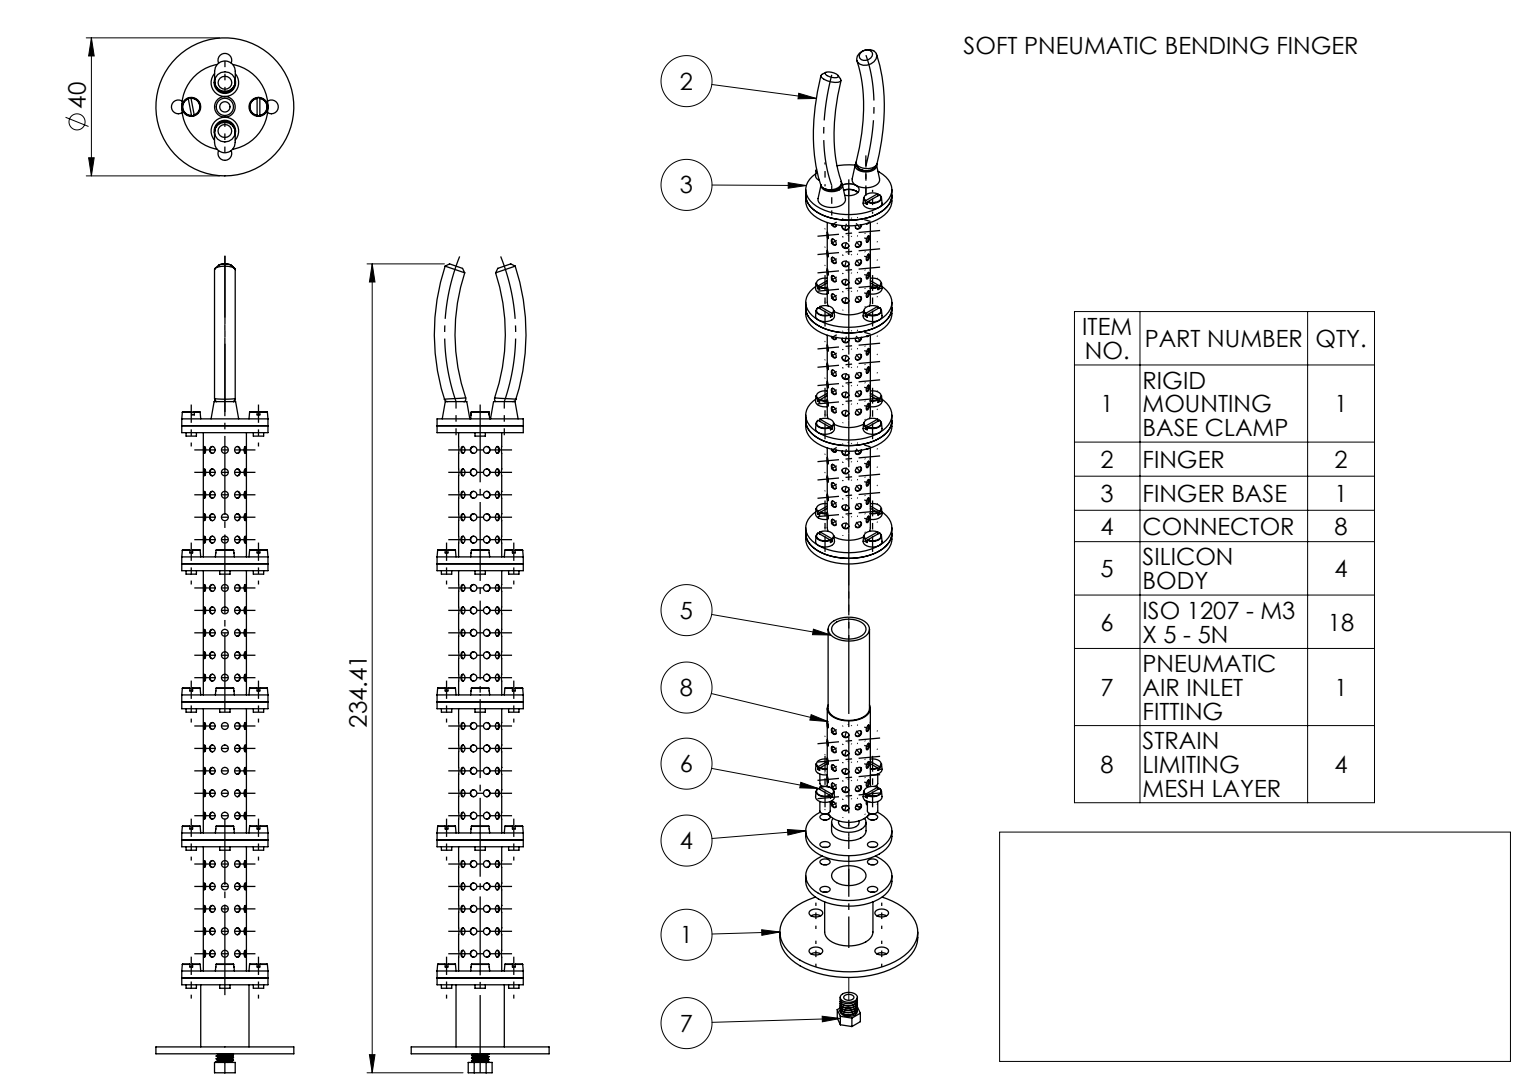
ISO-10303-21;
HEADER;
FILE_DESCRIPTION (('STEP AP214'),
    '1' );
FILE_NAME ('BR-012',
    '2026-10-04T10:31:01',
    ( '' ),
    ( '' ),
    'SwSTEP 2.0',
    'SolidWorks 2026',
    '' );
FILE_SCHEMA (( 'AUTOMOTIVE_DESIGN' ));
ENDSEC;

DATA;
#1 = DIRECTION ( 'NONE',  ( 1.251928832280965695E-16, 1.000000000000000000, 0.000000000000000000 ) ) ;
#2 = CARTESIAN_POINT ( 'NONE',  ( -5.408775798201173046, 2.598833957129639494, 10.88602261056916554 ) ) ;
#3 = CARTESIAN_POINT ( 'NONE',  ( 5.866817325727491372, 1.260653813892048003, 4.199777826161211536 ) ) ;
#4 = CARTESIAN_POINT ( 'NONE',  ( -5.621278735166248097, 2.101423246382425614, 30.02591947216899015 ) ) ;
#5 = ORIENTED_EDGE ( 'NONE', *, *, #943, .F. ) ;
#6 = ADVANCED_FACE ( 'NONE', ( #14827 ), #6324, .F. ) ;
#7 = VECTOR ( 'NONE', #2853, 1000.000000000000000 ) ;
#8 = ORIENTED_EDGE ( 'NONE', *, *, #4476, .T. ) ;
#9 = ORIENTED_EDGE ( 'NONE', *, *, #12350, .T. ) ;
#10 = LINE ( 'NONE', #5828, #1733 ) ;
#11 = EDGE_CURVE ( 'NONE', #6555, #15690, #9827, .T. ) ;
#12 = EDGE_LOOP ( 'NONE', ( #2014, #1529, #7352, #6634 ) ) ;
#13 = CARTESIAN_POINT ( 'NONE',  ( -1.461580736456472795, 1.461580736456472795, 1.150000001092474688 ) ) ;
#14 = DIRECTION ( 'NONE',  ( 0.000000000000000000, -0.000000000000000000, 1.000000000000000000 ) ) ;
#15 = DIRECTION ( 'NONE',  ( 0.000000000000000000, 1.000000000000000000, 0.000000000000000000 ) ) ;
#16 = CARTESIAN_POINT ( 'NONE',  ( 0.8561741729129460632, 185.8999999989075036, 9.066987299999999195 ) ) ;
#17 = CARTESIAN_POINT ( 'NONE',  ( 2.500000000000000000, 3.061616997868383141E-16, 2.100000000000000089 ) ) ;
#18 = LINE ( 'NONE', #14576, #2348 ) ;
#19 = ITEM_DEFINED_TRANSFORMATION ( 'NONE', 'NONE', #1959,  #14201 ) ;
#20 = FACE_OUTER_BOUND ( 'NONE', #6226, .T. ) ;
#21 = CARTESIAN_POINT ( 'NONE',  ( 0.8561741729129451750, 2.066987299999999639, 2.000000001092475443 ) ) ;
#22 = CARTESIAN_POINT ( 'NONE',  ( -3.061616997868391523E-16, 189.0000000000000000, -7.000000000000000000 ) ) ;
#23 = CARTESIAN_POINT ( 'NONE',  ( -2.191511056945971259, 226.6300844452854903, 5.385369267317587472 ) ) ;
#24 = CARTESIAN_POINT ( 'NONE',  ( 6.081836621194421255, 1.445163676684907417, 5.873058915543010627 ) ) ;
#25 = VERTEX_POINT ( 'NONE', #11007 ) ;
#26 = VERTEX_POINT ( 'NONE', #13779 ) ;
#27 = EDGE_LOOP ( 'NONE', ( #6618, #1977 ) ) ;
#28 = VERTEX_POINT ( 'NONE', #11082 ) ;
#29 = CARTESIAN_POINT ( 'NONE',  ( 8.572527594031473190E-16, 19.99999999999999645, 7.000000000000000000 ) ) ;
#30 = DIRECTION ( 'NONE',  ( 0.000000000000000000, 1.000000000000000000, 0.000000000000000000 ) ) ;
#31 = CARTESIAN_POINT ( 'NONE',  ( -2.499999999999998224, 185.2500000000000284, 8.035533905932741305 ) ) ;
#32 = CARTESIAN_POINT ( 'NONE',  ( -6.176542424588117974, 0.9554180641285662245, 31.13234125634169658 ) ) ;
#33 = CARTESIAN_POINT ( 'NONE',  ( -2.500000000000000444, 185.8999999978150584, 7.000000000000000000 ) ) ;
#34 = CARTESIAN_POINT ( 'NONE',  ( -3.107583187530418289, -5.133966411712689748, 12.37380682714709401 ) ) ;
#35 = CARTESIAN_POINT ( 'NONE',  ( -5.769755079862331826, 2.405651898698942581, 5.873058915543010627 ) ) ;
#36 = CARTESIAN_POINT ( 'NONE',  ( -6.176542424588075342, -0.9554180641288342324, 24.36765874365829987 ) ) ;
#37 = CARTESIAN_POINT ( 'NONE',  ( 0.9999502950804096679, -5.916088184763849789, 24.63108149190011176 ) ) ;
#38 = CARTESIAN_POINT ( 'NONE',  ( 0.000000000000000000, 22.00000000000000000, 0.000000000000000000 ) ) ;
#39 = CARTESIAN_POINT ( 'NONE',  ( -1.767766952966369320, 186.5999999978150754, 5.232233047033630235 ) ) ;
#40 = CARTESIAN_POINT ( 'NONE',  ( 2.467000123265670641, 227.8390626820829823, 8.944723654098295285 ) ) ;
#41 = FACE_BOUND ( 'NONE', #6027, .T. ) ;
#42 = EDGE_CURVE ( 'NONE', #14222, #12950, #1605, .T. ) ;
#43 = CARTESIAN_POINT ( 'NONE',  ( -2.367714804004699136, 189.3873339094368191, 5.166511778942795452 ) ) ;
#44 = EDGE_LOOP ( 'NONE', ( #13948, #7274 ) ) ;
#45 = CARTESIAN_POINT ( 'NONE',  ( 0.000000000000000000, 22.00000000000000000, -5.000000000000000000 ) ) ;
#46 = FACE_OUTER_BOUND ( 'NONE', #102, .T. ) ;
#47 = CARTESIAN_POINT ( 'NONE',  ( 7.799024015210693328, -1.482594289696895551, 24.49999999999999289 ) ) ;
#48 = LINE ( 'NONE', #2436, #232 ) ;
#49 = DIRECTION ( 'NONE',  ( -1.000000000000000000, 0.000000000000000000, 0.000000000000000000 ) ) ;
#50 = CARTESIAN_POINT ( 'NONE',  ( -3.420311045507875125, 4.931422832349270813, 10.49992038825521767 ) ) ;
#51 = EDGE_CURVE ( 'NONE', #13172, #10136, #3947, .T. ) ;
#52 = CARTESIAN_POINT ( 'NONE',  ( 1.461580736456473018, -1.461580736456472573, -0.6499999989075253559 ) ) ;
#53 = LINE ( 'NONE', #4919, #15568 ) ;
#54 = DIRECTION ( 'NONE',  ( 0.000000000000000000, 0.000000000000000000, 1.000000000000000000 ) ) ;
#55 = CARTESIAN_POINT ( 'NONE',  ( -1.767766952966369765, 186.8300000002185186, 8.767766952966368876 ) ) ;
#56 = CARTESIAN_POINT ( 'NONE',  ( -4.070051655338111196, 4.744673454622471809, 5.873673286359928802 ) ) ;
#57 = CARTESIAN_POINT ( 'NONE',  ( 1.989910900261709470, 228.2393533748197569, 6.930657055068108363 ) ) ;
#58 = CARTESIAN_POINT ( 'NONE',  ( 0.8561741729129452860, 2.066987299999999639, 2.000000001092474999 ) ) ;
#59 = VECTOR ( 'NONE', #8000, 1000.000000000000000 ) ;
#60 = CARTESIAN_POINT ( 'NONE',  ( 5.558508435838322548, -2.857531096718671115, 24.49999999999999289 ) ) ;
#61 = ORIENTED_EDGE ( 'NONE', *, *, #6502, .F. ) ;
#62 = DIRECTION ( 'NONE',  ( -0.5877852522924685852, -0.8090169943749507819, 0.000000000000000000 ) ) ;
#63 = PRODUCT_DEFINITION_SHAPE ( 'NONE', 'NONE',  #15745 ) ;
#64 = CARTESIAN_POINT ( 'NONE',  ( -0.8561741729129470624, 185.5999999989075206, 9.066987300000000971 ) ) ;
#65 = DIRECTION ( 'NONE',  ( 1.000000000000000000, 0.000000000000000000, 0.000000000000000000 ) ) ;
#67 = ORIENTED_EDGE ( 'NONE', *, *, #457, .F. ) ;
#66 = CARTESIAN_POINT ( 'NONE',  ( 3.566234721238059624, 5.134387337253815353, 30.00008258189710730 ) ) ;
#68 = EDGE_CURVE ( 'NONE', #7891, #15426, #13595, .T. ) ;
#69 = CARTESIAN_POINT ( 'NONE',  ( 0.6151877315911880029, -6.220340188095996758, 25.29906673469669443 ) ) ;
#70 = EDGE_CURVE ( 'NONE', #13541, #6298, #6755, .T. ) ;
#71 = CARTESIAN_POINT ( 'NONE',  ( 2.817313151350924638, 5.579000502529565253, 24.49999999999999289 ) ) ;
#72 = DIRECTION ( 'NONE',  ( -0.5877852522924685852, -0.8090169943749508930, 0.000000000000000000 ) ) ;
#73 = CARTESIAN_POINT ( 'NONE',  ( -1.732476358310940601, 189.0000000000000853, 8.805961798289683173 ) ) ;
#74 = CARTESIAN_POINT ( 'NONE',  ( 4.005785023174416537, -4.467917056767432449, 18.79952054102714243 ) ) ;
#75 = CARTESIAN_POINT ( 'NONE',  ( -2.500000000000000000, 0.000000000000000000, -2.199999997815050623 ) ) ;
#76 = CARTESIAN_POINT ( 'NONE',  ( -0.9737778612005270062, -5.920671847850523584, 30.73736375884650585 ) ) ;
#77 = LINE ( 'NONE', #5895, #15592 ) ;
#78 = EDGE_CURVE ( 'NONE', #4035, #7910, #13252, .T. ) ;
#79 = CARTESIAN_POINT ( 'NONE',  ( -0.9740012993918838458, -6.173846968979659344, 18.26164920628437471 ) ) ;
#80 = CYLINDRICAL_SURFACE ( 'NONE', #3453, 2.000000000000000000 ) ;
#81 = CARTESIAN_POINT ( 'NONE',  ( 0.000000000000000000, 0.000000000000000000, -5.500000000000000000 ) ) ;
#82 = ORIENTED_EDGE ( 'NONE', *, *, #7980, .T. ) ;
#83 = B_SPLINE_CURVE_WITH_KNOTS ( 'NONE', 3,
 ( #5175, #14802, #5099, #8688, #8760, #13593, #1502, #6378, #11290, #544, #7481, #9951, #10027, #7789, #7554, #1580, #2625, #11212 ),
 .UNSPECIFIED., .F., .F.,
 ( 4, 2, 2, 2, 2, 2, 2, 2, 4 ),
 ( 0.000000000000000000, 0.0003914898357794967363, 0.0007829796715589934725, 0.001174469507338490263, 0.001565959343117986945, 0.001957449178897483627, 0.002348939014676980526, 0.002740428850456476991, 0.003131918686235973890 ),
 .UNSPECIFIED. ) ;
#84 = ORIENTED_EDGE ( 'NONE', *, *, #4688, .F. ) ;
#85 = ORIENTED_EDGE ( 'NONE', *, *, #14143, .F. ) ;
#86 = CARTESIAN_POINT ( 'NONE',  ( -2.692215568229989753, 5.362327947133520567, 24.76229037835931734 ) ) ;
#87 = ORIENTED_EDGE ( 'NONE', *, *, #14600, .T. ) ;
#88 = CARTESIAN_POINT ( 'NONE',  ( -1.035533905932737753, 2.500000000000000444, -1.549999997815050490 ) ) ;
#89 = CARTESIAN_POINT ( 'NONE',  ( 5.903472034603520768, 2.056448723545130974, 19.00008219321555103 ) ) ;
#90 = CARTESIAN_POINT ( 'NONE',  ( 6.106056299406735555, 1.336851112280737386, 31.79887838423339730 ) ) ;
#91 = CARTESIAN_POINT ( 'NONE',  ( -1.461580736456473018, 188.7499999989075263, 5.538419263543527649 ) ) ;
#92 = EDGE_CURVE ( 'NONE', #15044, #5826, #4325, .T. ) ;
#93 = AXIS2_PLACEMENT_3D ( 'NONE', #6041, #2604, #1097 ) ;
#94 = CARTESIAN_POINT ( 'NONE',  ( -1.530808498934191571E-16, 2.500000000000000000, 0.6999999999999998446 ) ) ;
#95 = LINE ( 'NONE', #7268, #828 ) ;
#96 = CONTEXT_DEPENDENT_SHAPE_REPRESENTATION ( #10266, #5907 ) ;
#97 = CARTESIAN_POINT ( 'NONE',  ( 3.421280866381150698, 4.930711975950905490, 6.000049320733126024 ) ) ;
#98 = CARTESIAN_POINT ( 'NONE',  ( 2.066987299999999639, 0.8561741729129456191, -2.299999998907525711 ) ) ;
#99 = CARTESIAN_POINT ( 'NONE',  ( 4.435347140101059793, -4.403429997944484420, 30.86762589283693714 ) ) ;
#100 = CARTESIAN_POINT ( 'NONE',  ( -2.809196860006122787, 226.9495188873497966, 6.326437523183426670 ) ) ;
#101 = DIRECTION ( 'NONE',  ( 0.000000000000000000, 0.000000000000000000, -1.000000000000000000 ) ) ;
#102 = EDGE_LOOP ( 'NONE', ( #11466, #15646, #12937, #12328 ) ) ;
#103 = EDGE_LOOP ( 'NONE', ( #8397, #1444 ) ) ;
#104 = EDGE_LOOP ( 'NONE', ( #9975, #181, #5986, #469 ) ) ;
#105 = CARTESIAN_POINT ( 'NONE',  ( 1.354942165200771727E-13, 6.000000000000000888, 16.99999999999998579 ) ) ;
#106 = CARTESIAN_POINT ( 'NONE',  ( 1.753917783834456179, 189.0000000000000568, 8.787807858281036388 ) ) ;
#107 = CARTESIAN_POINT ( 'NONE',  ( 7.347880431581855163E-16, -6.250000000000000888, 4.000000000000004441 ) ) ;
#108 = CARTESIAN_POINT ( 'NONE',  ( 3.010624175977998807, -5.190832888732208161, 12.29888242247939623 ) ) ;
#109 = VECTOR ( 'NONE', #6035, 1000.000000000000114 ) ;
#110 = UNCERTAINTY_MEASURE_WITH_UNIT (LENGTH_MEASURE( 1.000000000000000082E-05 ), #6665, 'distance_accuracy_value', 'NONE');
#111 = CARTESIAN_POINT ( 'NONE',  ( 0.5042987395408317086, 5.979983180450071600, 12.37329304179975509 ) ) ;
#112 = CARTESIAN_POINT ( 'NONE',  ( -0.2637975869345823843, -6.245592211692903462, 25.47332839949191197 ) ) ;
#113 = EDGE_CURVE ( 'NONE', #5247, #7816, #14877, .T. ) ;
#114 = CARTESIAN_POINT ( 'NONE',  ( -5.858813228503674253, 2.179803269293212331, 5.973772828752684561 ) ) ;
#115 = CARTESIAN_POINT ( 'NONE',  ( 5.931828553037963303, 0.9033193133619970006, 30.73805675996854703 ) ) ;
#116 = DIRECTION ( 'NONE',  ( -6.123233995736766036E-17, 1.000000000000000000, 0.000000000000000000 ) ) ;
#117 = CARTESIAN_POINT ( 'NONE',  ( 0.000000000000000000, 102.0000000000000142, 0.000000000000000000 ) ) ;
#118 = CARTESIAN_POINT ( 'NONE',  ( -7.826584432629735133E-16, 189.2999999978150356, 9.500000000000001776 ) ) ;
#119 = CARTESIAN_POINT ( 'NONE',  ( 1.829800800964088481, 226.5245823332902546, 5.074452397578279594 ) ) ;
#120 = CARTESIAN_POINT ( 'NONE',  ( 5.866817325727508248, 1.260653813891974062, 10.69977782616119732 ) ) ;
#121 = CARTESIAN_POINT ( 'NONE',  ( -2.425137606382978372, 188.9999999978561505, 7.628313597219490205 ) ) ;
#122 = EDGE_LOOP ( 'NONE', ( #8457, #957, #1817, #14670 ) ) ;
#123 = CARTESIAN_POINT ( 'NONE',  ( -3.735642931251032639, 4.696778275484473575, 5.974080527831013399 ) ) ;
#124 = DIRECTION ( 'NONE',  ( -0.3090169943749584980, 0.9510565162951498674, 0.000000000000000000 ) ) ;
#125 = CARTESIAN_POINT ( 'NONE',  ( 0.000000000000000000, 6.250000000000000888, 25.49999999999999645 ) ) ;
#126 = CARTESIAN_POINT ( 'NONE',  ( 0.5031281619709804254, 5.980084330432649864, 23.62602272744524967 ) ) ;
#127 = CARTESIAN_POINT ( 'NONE',  ( 0.000000000000000000, 184.0000000000000000, 0.000000000000000000 ) ) ;
#128 = CARTESIAN_POINT ( 'NONE',  ( -2.782769401326250058, 5.315896561274810139, 10.99571079637980553 ) ) ;
#129 = CARTESIAN_POINT ( 'NONE',  ( 3.796994071234844259E-16, -2.066987299999999639, 0.8500000010924748661 ) ) ;
#130 = CARTESIAN_POINT ( 'NONE',  ( 5.621197618055712830, -2.101623592078416980, 4.026019798777604741 ) ) ;
#131 = AXIS2_PLACEMENT_3D ( 'NONE', #7436, #13712, #10064 ) ;
#132 = LINE ( 'NONE', #11034, #13057 ) ;
#133 = CARTESIAN_POINT ( 'NONE',  ( -2.500000000000000444, 186.7300000002184959, 7.000000000000000000 ) ) ;
#134 = CARTESIAN_POINT ( 'NONE',  ( -2.500000000000000000, 0.000000000000000000, -2.199999997815050623 ) ) ;
#135 = CARTESIAN_POINT ( 'NONE',  ( 0.000000000000000000, 2.000000000000000000, -5.000000000000000000 ) ) ;
#136 = CARTESIAN_POINT ( 'NONE',  ( 0.8561741729129452860, 2.066987299999999639, -1.199999998907525178 ) ) ;
#137 = CARTESIAN_POINT ( 'NONE',  ( 0.7995298244854847081, 5.947211616899245712, 31.61456014619858834 ) ) ;
#138 = EDGE_LOOP ( 'NONE', ( #2074, #6168, #2631, #14050 ) ) ;
#139 = CARTESIAN_POINT ( 'NONE',  ( 0.8561741729129465073, -2.066987299999999195, 0.7000000010924749549 ) ) ;
#140 = CARTESIAN_POINT ( 'NONE',  ( -1.461580736456473906, 186.3499999989074922, 8.461580736456474128 ) ) ;
#141 = CARTESIAN_POINT ( 'NONE',  ( -4.290821322214377176, -4.545321419741554791, 12.11441947245482886 ) ) ;
#142 = VECTOR ( 'NONE', #3301, 1000.000000000000114 ) ;
#144 = ORIENTED_EDGE ( 'NONE', *, *, #8868, .F. ) ;
#143 = CARTESIAN_POINT ( 'NONE',  ( 8.809142651444723526E-17, 184.6499999989075320, 4.933012699999999029 ) ) ;
#145 = CYLINDRICAL_SURFACE ( 'NONE', #13956, 1.000000000000000888 ) ;
#146 = LINE ( 'NONE', #13353, #5536 ) ;
#147 = DIRECTION ( 'NONE',  ( -1.000000000000000000, 0.000000000000000000, 0.000000000000000000 ) ) ;
#148 = B_SPLINE_CURVE_WITH_KNOTS ( 'NONE', 1,
 ( #12898, #4831 ),
 .UNSPECIFIED., .F., .F.,
 ( 2, 2 ),
 ( 0.000000000000000000, 1.000000000000000000 ),
 .UNSPECIFIED. ) ;
#149 = DIRECTION ( 'NONE',  ( 0.8090169943749421222, 0.5877852522924802425, 0.000000000000000000 ) ) ;
#150 = CARTESIAN_POINT ( 'NONE',  ( 1.461580736456472573, 188.9499999989075150, 8.461580736456474128 ) ) ;
#151 = CARTESIAN_POINT ( 'NONE',  ( 5.782895619916224028, -1.604017620857841386, 25.47408052783099919 ) ) ;
#152 = CARTESIAN_POINT ( 'NONE',  ( -13.50000000000000000, -0.001000000000000132727, -1.999999999999997113 ) ) ;
#153 = CARTESIAN_POINT ( 'NONE',  ( -1.000079958708118610, -5.916066267613704355, 31.13152738882033788 ) ) ;
#154 = CARTESIAN_POINT ( 'NONE',  ( 5.621197618055728817, -2.101623592078373903, 10.52601979877759142 ) ) ;
#155 = CARTESIAN_POINT ( 'NONE',  ( -4.435347140101089103, 4.403429997944455110, 31.00000000000000000 ) ) ;
#156 = CARTESIAN_POINT ( 'NONE',  ( 12.50000000000000533, 1.530808498934192113E-15, 0.000000000000000000 ) ) ;
#157 = CARTESIAN_POINT ( 'NONE',  ( -5.935543223013860725, 0.8771126767606856056, 30.86760611998365178 ) ) ;
#158 = EDGE_CURVE ( 'NONE', #3364, #642, #4897, .T. ) ;
#159 = VERTEX_POINT ( 'NONE', #1682 ) ;
#160 = EDGE_CURVE ( 'NONE', #4150, #13293, #5091, .T. ) ;
#161 = ORIENTED_EDGE ( 'NONE', *, *, #15144, .T. ) ;
#162 = ORIENTED_EDGE ( 'NONE', *, *, #10171, .F. ) ;
#163 = CARTESIAN_POINT ( 'NONE',  ( -5.329907877631262281, -2.755840666746435019, 24.76194324003146008 ) ) ;
#164 = VECTOR ( 'NONE', #7946, 1000.000000000000000 ) ;
#165 = ORIENTED_EDGE ( 'NONE', *, *, #10559, .T. ) ;
#166 = PRODUCT ( 'finger base', 'finger base', '', ( #15382 ) ) ;
#167 = CARTESIAN_POINT ( 'NONE',  ( -1.461580736456472351, -1.461580736456473018, -0.2499999989075251672 ) ) ;
#168 = FACE_BOUND ( 'NONE', #3506, .T. ) ;
#169 = DIRECTION ( 'NONE',  ( 0.000000000000000000, 0.000000000000000000, 1.000000000000000000 ) ) ;
#170 = DIRECTION ( 'NONE',  ( -1.000000000000000000, 3.326610055774637112E-18, 1.062480551894331163E-17 ) ) ;
#171 = CARTESIAN_POINT ( 'NONE',  ( 1.767766952966369320, -1.767766952966368654, 2.000000000000000000 ) ) ;
#172 = CARTESIAN_POINT ( 'NONE',  ( -5.558508435838229289, 2.857531096718854524, 5.000000000000004441 ) ) ;
#173 = CONTEXT_DEPENDENT_SHAPE_REPRESENTATION ( #5992, #5517 ) ;
#174 = CARTESIAN_POINT ( 'NONE',  ( 2.668367453516629517, 5.373994336898131330, 5.130649613488545313 ) ) ;
#175 = CARTESIAN_POINT ( 'NONE',  ( 2.066987300000000083, -0.8561741729129449530, -0.7999999989075252671 ) ) ;
#176 = CARTESIAN_POINT ( 'NONE',  ( 0.000000000000000000, 0.000000000000000000, 5.000000000000004441 ) ) ;
#177 = CARTESIAN_POINT ( 'NONE',  ( -2.923025936753522291, 227.5090509392885281, 7.973756422523831766 ) ) ;
#178 = EDGE_CURVE ( 'NONE', #5942, #5121, #706, .T. ) ;
#179 = ORIENTED_EDGE ( 'NONE', *, *, #8379, .T. ) ;
#180 = ORIENTED_EDGE ( 'NONE', *, *, #12545, .T. ) ;
#181 = ORIENTED_EDGE ( 'NONE', *, *, #13568, .T. ) ;
#182 = DIRECTION ( 'NONE',  ( -0.1736481776669306920, -0.9848077530122080203, 0.000000000000000000 ) ) ;
#183 = LINE ( 'NONE', #11083, #4538 ) ;
#184 = B_SPLINE_CURVE_WITH_KNOTS ( 'NONE', 3,
 ( #1419, #11210, #385, #5255, #7552, #10102, #6529, #6608, #14955, #11441, #11134, #235, #4046, #5097, #5411, #8917, #12556, #1655 ),
 .UNSPECIFIED., .F., .F.,
 ( 4, 2, 2, 2, 2, 2, 2, 2, 4 ),
 ( 0.003131918686235975625, 0.003523310662250265894, 0.003914702638264556597, 0.004306094614278846433, 0.004697486590293137136, 0.005088878566307427839, 0.005480270542321717675, 0.005871662518336007511, 0.006263054494350298214 ),
 .UNSPECIFIED. ) ;
#185 = CARTESIAN_POINT ( 'NONE',  ( 6.123233995736766282E-16, -6.000000000000000888, 6.000000000000005329 ) ) ;
#186 = CARTESIAN_POINT ( 'NONE',  ( 0.1306394121200732117, -6.249999999999998224, 16.99999999999998934 ) ) ;
#187 = DIRECTION ( 'NONE',  ( 0.8660254037844385966, 0.4999999999999998890, 0.000000000000000000 ) ) ;
#188 = DIRECTION ( 'NONE',  ( 0.000000000000000000, 0.000000000000000000, 1.000000000000000000 ) ) ;
#189 = DIRECTION ( 'NONE',  ( -0.5877852522924685852, -0.8090169943749508930, 0.000000000000000000 ) ) ;
#190 = CARTESIAN_POINT ( 'NONE',  ( 5.486982057989218120, -2.429327048029818137, 12.29931806258173488 ) ) ;
#191 = CARTESIAN_POINT ( 'NONE',  ( -7.799024015210622274, -1.482594289697344969, 17.99999999999998934 ) ) ;
#192 = CARTESIAN_POINT ( 'NONE',  ( 6.805491029613696752E-14, 66.00000000000000000, -9.750000000000003553 ) ) ;
#193 = B_SPLINE_CURVE_WITH_KNOTS ( 'NONE', 3,
 ( #6450, #7867, #11284, #4121, #12707, #459, #1650 ),
 .UNSPECIFIED., .F., .F.,
 ( 4, 3, 4 ),
 ( 0.004471049636504374758, 0.004805482912052319762, 0.005232732616948215093 ),
 .UNSPECIFIED. ) ;
#194 = CARTESIAN_POINT ( 'NONE',  ( 4.404571325722361763E-17, 185.7699999975965568, 4.500000000000000000 ) ) ;
#195 = CARTESIAN_POINT ( 'NONE',  ( -1.740752211025599738, 227.9442165381023528, 6.078285037125840340 ) ) ;
#196 = CARTESIAN_POINT ( 'NONE',  ( 2.789580270747262780, 227.6450226773988845, 8.373868502673408543 ) ) ;
#197 = CARTESIAN_POINT ( 'NONE',  ( 0.3061381340472814627, 189.0451911194899424, 10.17413847366682234 ) ) ;
#198 =( REPRESENTATION_RELATIONSHIP ('NONE','NONE', #11191, #3660 ) REPRESENTATION_RELATIONSHIP_WITH_TRANSFORMATION ( #14497 )SHAPE_REPRESENTATION_RELATIONSHIP( ) );
#199 = CIRCLE ( 'NONE', #5549, 2.499999999999999556 ) ;
#200 = CARTESIAN_POINT ( 'NONE',  ( -0.2618185962740512407, 189.0446530151151023, 10.17853758010602760 ) ) ;
#201 = EDGE_CURVE ( 'NONE', #13777, #13408, #2146, .T. ) ;
#202 = VERTEX_POINT ( 'NONE', #2611 ) ;
#203 = CARTESIAN_POINT ( 'NONE',  ( -6.176542424588105540, -0.9554180641286327269, 5.000000000000004441 ) ) ;
#204 = CARTESIAN_POINT ( 'NONE',  ( -5.859221468178929193, 2.178708437343280568, 23.52591457665828401 ) ) ;
#205 = PRODUCT_RELATED_PRODUCT_CATEGORY ( 'part', '', ( #166 ) ) ;
#206 = CARTESIAN_POINT ( 'NONE',  ( -12.50000000000000533, 0.000000000000000000, 2.000000000000001776 ) ) ;
#207 = CARTESIAN_POINT ( 'NONE',  ( 6.176542424588116198, 0.9554180641285651143, 11.63060690723497537 ) ) ;
#208 = CARTESIAN_POINT ( 'NONE',  ( 0.9639874461523436633, 228.2061259459514133, 10.02419290002115915 ) ) ;
#209 =( BOUNDED_CURVE ( )  B_SPLINE_CURVE ( 2, ( #7437, #5274, #15205, #1752, #11093, #14680, #10274, #6626, #3769 ),
 .UNSPECIFIED., .F., .F. ) 
 B_SPLINE_CURVE_WITH_KNOTS ( ( 3, 2, 2, 2, 3 ),
 ( 0.000000000000000000, 0.01785714285714285615, 0.03571428571428571230, 0.05357142857142856845, 0.07142857142857142461 ),
 .UNSPECIFIED. ) 
 CURVE ( )  GEOMETRIC_REPRESENTATION_ITEM ( )  RATIONAL_B_SPLINE_CURVE ( ( 1.000000000000000000, 0.9238795325112867385, 1.000000000000000000, 0.9238795325112867385, 1.000000000000000000, 0.9238795325112867385, 1.000000000000000000, 0.9238795325112867385, 1.000000000000000000 ) ) 
 REPRESENTATION_ITEM ( '' )  );
#210 = EDGE_CURVE ( 'NONE', #4790, #898, #15357, .T. ) ;
#211 = AXIS2_PLACEMENT_3D ( 'NONE', #13271, #4928, #12230 ) ;
#212 = CARTESIAN_POINT ( 'NONE',  ( 4.322356511625485176, 7.650514973136679941, 24.49999999999999289 ) ) ;
#213 = CARTESIAN_POINT ( 'NONE',  ( 0.8561741729129451750, 2.066987299999999639, -1.199999998907525622 ) ) ;
#214 = FACE_OUTER_BOUND ( 'NONE', #10362, .T. ) ;
#215 = SURFACE_SIDE_STYLE ('',( #11110 ) ) ;
#216 = CARTESIAN_POINT ( 'NONE',  ( -0.6144300524833441468, -6.220417338033054300, 30.20033372175933550 ) ) ;
#217 = CARTESIAN_POINT ( 'NONE',  ( -2.500000000000000444, 186.7800000002184504, 8.035533905932737753 ) ) ;
#218 = DIRECTION ( 'NONE',  ( 0.000000000000000000, 0.000000000000000000, -1.000000000000000000 ) ) ;
#219 = CARTESIAN_POINT ( 'NONE',  ( 0.8799020092372641377, 228.8451675208714562, 8.680282862240067843 ) ) ;
#220 = CARTESIAN_POINT ( 'NONE',  ( -0.8561741729129455081, 2.066987299999999639, -1.899999998907525134 ) ) ;
#221 = CARTESIAN_POINT ( 'NONE',  ( -3.567624405365271478, -5.133384272590760133, 10.50004921015705150 ) ) ;
#222 = CARTESIAN_POINT ( 'NONE',  ( -1.265664690411614835E-16, 2.066987299999999639, 0.2500000010924746663 ) ) ;
#223 = VECTOR ( 'NONE', #5063, 1000.000000000000114 ) ;
#224 = CARTESIAN_POINT ( 'NONE',  ( -2.066987300000001859, 187.8999999989075036, 7.856174172912944620 ) ) ;
#225 = CARTESIAN_POINT ( 'NONE',  ( 6.172651332693116721, -0.9815532474592382206, 18.26190213084011660 ) ) ;
#226 = EDGE_LOOP ( 'NONE', ( #14083, #11757, #15041, #247 ) ) ;
#227 = CARTESIAN_POINT ( 'NONE',  ( -3.735642931251134335, -4.696778275484388310, 23.52591947216897594 ) ) ;
#228 = CARTESIAN_POINT ( 'NONE',  ( -11.25000000000000355, 3.419666426228851687E-14, 2.000000000000001776 ) ) ;
#229 = CARTESIAN_POINT ( 'NONE',  ( 5.903596343266298341, -2.055998103990583026, 31.99995078984293428 ) ) ;
#230 = CARTESIAN_POINT ( 'NONE',  ( 5.131373506000437068, 7.062729720844210135, 24.49999999999999289 ) ) ;
#231 = CARTESIAN_POINT ( 'NONE',  ( -0.8561741729129471734, 188.7999999989075093, 9.066987300000000971 ) ) ;
#232 = VECTOR ( 'NONE', #9608, 1000.000000000000000 ) ;
#233 = CARTESIAN_POINT ( 'NONE',  ( -0.05280792143845736142, 189.0000000000001137, 9.499442202459045248 ) ) ;
#234 = CARTESIAN_POINT ( 'NONE',  ( 9.750000000000003553, 19.99999999999999645, 1.020968533498575335E-13 ) ) ;
#235 = CARTESIAN_POINT ( 'NONE',  ( 3.922396193919112317, -4.541970110199391009, 5.873806827147107334 ) ) ;
#236 = CARTESIAN_POINT ( 'NONE',  ( -5.746837578676007752, 1.729433780394243003, 10.50004946353775459 ) ) ;
#237 = CYLINDRICAL_SURFACE ( 'NONE', #3717, 2.500000000000000000 ) ;
#238 = CARTESIAN_POINT ( 'NONE',  ( 13.50000000000000000, 2.000000000000000000, -2.000000000000000444 ) ) ;
#239 = ORIENTED_EDGE ( 'NONE', *, *, #1750, .T. ) ;
#240 = CARTESIAN_POINT ( 'NONE',  ( -0.8561741729129455081, 187.0999999989075206, 4.933012699999999029 ) ) ;
#241 = ORIENTED_EDGE ( 'NONE', *, *, #4453, .T. ) ;
#242 = PLANE ( 'NONE',  #13414 ) ;
#243 = ORIENTED_EDGE ( 'NONE', *, *, #15436, .T. ) ;
#244 = AXIS2_PLACEMENT_3D ( 'NONE', #12080, #1179, #6133 ) ;
#245 = CARTESIAN_POINT ( 'NONE',  ( -2.782713018890816681, 5.315928322779066129, 25.00439760644211518 ) ) ;
#246 = CIRCLE ( 'NONE', #4794, 1.499999999999999556 ) ;
#247 = ORIENTED_EDGE ( 'NONE', *, *, #524, .F. ) ;
#248 = CARTESIAN_POINT ( 'NONE',  ( 3.796994071234844259E-16, -2.066987299999999639, -0.1499999989075253282 ) ) ;
#249 = CARTESIAN_POINT ( 'NONE',  ( 5.770288754215144422, 2.404361317819916355, 18.87381964045070859 ) ) ;
#250 = CARTESIAN_POINT ( 'NONE',  ( -2.113934160113910998, 227.9745842263959048, 9.343330332359114365 ) ) ;
#251 = CARTESIAN_POINT ( 'NONE',  ( -0.8561741729129470624, 188.9999999989074979, 9.066987299999999195 ) ) ;
#252 = CARTESIAN_POINT ( 'NONE',  ( 0.4831378333609244180, 2.500000000000000000, -2.516327958217759342 ) ) ;
#253 = ADVANCED_FACE ( 'NONE', ( #9289 ), #846, .F. ) ;
#254 = DIRECTION ( 'NONE',  ( 0.000000000000000000, 1.000000000000000000, 0.000000000000000000 ) ) ;
#255 = DIRECTION ( 'NONE',  ( 0.8090169943749421222, 0.5877852522924802425, 0.000000000000000000 ) ) ;
#256 = CARTESIAN_POINT ( 'NONE',  ( 3.796994071234844259E-16, -2.066987299999999639, 0.8500000010924748661 ) ) ;
#257 = CARTESIAN_POINT ( 'NONE',  ( -6.155867707731118799, 1.081837891425841747, 30.49563030319847101 ) ) ;
#258 = CARTESIAN_POINT ( 'NONE',  ( -2.548338711267991386, 226.7802694665861338, 5.827877803219676522 ) ) ;
#259 = ORIENTED_EDGE ( 'NONE', *, *, #5440, .T. ) ;
#260 = VERTEX_POINT ( 'NONE', #5788 ) ;
#261 = ORIENTED_EDGE ( 'NONE', *, *, #6781, .F. ) ;
#262 = CARTESIAN_POINT ( 'NONE',  ( 5.330189595673648917, -2.755293208590215315, 30.73617396794403689 ) ) ;
#263 = CARTESIAN_POINT ( 'NONE',  ( 4.153440676704428292, 4.671190581744466108, 4.200455375311575423 ) ) ;
#264 = ORIENTED_EDGE ( 'NONE', *, *, #8261, .T. ) ;
#265 = CARTESIAN_POINT ( 'NONE',  ( -6.155854678529451895, -1.081900940642234854, 17.49574050496990552 ) ) ;
#266 = CARTESIAN_POINT ( 'NONE',  ( -2.849573632035295567, -5.280958870664590243, 18.61561732698604743 ) ) ;
#267 = EDGE_CURVE ( 'NONE', #4415, #8748, #895, .T. ) ;
#268 = CARTESIAN_POINT ( 'NONE',  ( 3.254737477227910514, -5.337033878705263135, 23.62632671364006498 ) ) ;
#269 = CARTESIAN_POINT ( 'NONE',  ( 1.035533905932737975, 184.8499999978150754, 4.500000000000000888 ) ) ;
#270 = CARTESIAN_POINT ( 'NONE',  ( -3.159082487394833105, 5.393634094348302099, 10.70045537531157365 ) ) ;
#271 = CARTESIAN_POINT ( 'NONE',  ( 1.000049560716759212, -5.916071405810109596, 24.36967799011533131 ) ) ;
#272 = SHAPE_DEFINITION_REPRESENTATION ( #8433, #11191 ) ;
#273 = CARTESIAN_POINT ( 'NONE',  ( 1.767766952966369320, 185.6699999975965625, 5.232233047033630235 ) ) ;
#274 = CARTESIAN_POINT ( 'NONE',  ( 0.1304739971030711432, 227.6100227634930775, 5.113114354890055502 ) ) ;
#275 = EDGE_CURVE ( 'NONE', #9042, #302, #14114, .T. ) ;
#276 = CARTESIAN_POINT ( 'NONE',  ( -2.974673115704016713, 227.4156934420934419, 7.698994310615434600 ) ) ;
#277 = CARTESIAN_POINT ( 'NONE',  ( -2.345330793980067607, 188.9999999986873149, 6.116719614743881372 ) ) ;
#278 = VERTEX_POINT ( 'NONE', #3158 ) ;
#279 = CARTESIAN_POINT ( 'NONE',  ( -4.005361199354998014, 4.468319061418771554, 5.800222173838807116 ) ) ;
#280 = DIRECTION ( 'NONE',  ( -6.123233995736766036E-17, 1.000000000000000000, 0.000000000000000000 ) ) ;
#281 = CARTESIAN_POINT ( 'NONE',  ( -3.420311045507988368, 4.931422832349193541, 23.49992038825522656 ) ) ;
#282 = CARTESIAN_POINT ( 'NONE',  ( 1.500000000000000000, -9.750000000000003553, 2.000000000000001776 ) ) ;
#283 = CARTESIAN_POINT ( 'NONE',  ( 3.000012661665197200, 227.2854160473209504, 7.315512558684322819 ) ) ;
#284 = CARTESIAN_POINT ( 'NONE',  ( -4.344762547369668049, -4.493114738039260203, 31.50308643866046054 ) ) ;
#285 = AXIS2_PLACEMENT_3D ( 'NONE', #127, #3629, #8659 ) ;
#286 = CARTESIAN_POINT ( 'NONE',  ( -0.8561741729129455081, 2.066987299999999639, -1.899999998907525134 ) ) ;
#287 = CARTESIAN_POINT ( 'NONE',  ( -3.255013540813805673, 5.336859797930734395, 23.62618035954928786 ) ) ;
#288 =( NAMED_UNIT ( * ) SI_UNIT ( $, .STERADIAN. ) SOLID_ANGLE_UNIT ( ) );
#289 = ADVANCED_FACE ( 'NONE', ( #4509 ), #10713, .T. ) ;
#290 = CARTESIAN_POINT ( 'NONE',  ( 5.665707375537430757, 1.979196487016795292, 6.000079611744768115 ) ) ;
#291 = CARTESIAN_POINT ( 'NONE',  ( -2.500000000000000444, 186.7500000000000000, 5.964466094067261359 ) ) ;
#292 = FACE_OUTER_BOUND ( 'NONE', #8134, .T. ) ;
#293 = CARTESIAN_POINT ( 'NONE',  ( -0.2610185499608090876, 227.6142484773064325, 5.125318457402467942 ) ) ;
#294 = LINE ( 'NONE', #13810, #11835 ) ;
#295 = B_SPLINE_CURVE_WITH_KNOTS ( 'NONE', 3,
 ( #10005, #367, #7304, #7609, #8735, #12457, #14777, #9696, #13567, #2677, #130, #7529, #13493, #1395, #2441, #6195, #14533, #1557 ),
 .UNSPECIFIED., .F., .F.,
 ( 4, 2, 2, 2, 2, 2, 2, 2, 4 ),
 ( 0.003131918686235955242, 0.003523310662250247680, 0.003914702638264540117, 0.004306094614278832555, 0.004697486590293124993, 0.005088878566307417431, 0.005480270542321709869, 0.005871662518336002307, 0.006263054494350294744 ),
 .UNSPECIFIED. ) ;
#296 = CARTESIAN_POINT ( 'NONE',  ( 2.817313151351047207, 5.579000502529503080, 11.63063932754212892 ) ) ;
#297 = CYLINDRICAL_SURFACE ( 'NONE', #14167, 1.499999999999999556 ) ;
#298 = AXIS2_PLACEMENT_3D ( 'NONE', #11149, #8855, #14815 ) ;
#299 = CARTESIAN_POINT ( 'NONE',  ( -1.965116437629976787E-16, 189.2499999989075263, 4.933012699999999029 ) ) ;
#300 = CARTESIAN_POINT ( 'NONE',  ( 5.858736126997204252, -2.179962889276876314, 18.97359571723300320 ) ) ;
#302 = VERTEX_POINT ( 'NONE', #12936 ) ;
#301 = CARTESIAN_POINT ( 'NONE',  ( -2.066987300000000971, 188.0999999989074922, 7.856174172912944620 ) ) ;
#303 = CARTESIAN_POINT ( 'NONE',  ( -3.735642931251081489, -4.696778275484434495, 17.02591947216898305 ) ) ;
#304 = DIRECTION ( 'NONE',  ( 0.000000000000000000, 0.000000000000000000, 1.000000000000000000 ) ) ;
#305 = B_SPLINE_CURVE_WITH_KNOTS ( 'NONE', 3,
 ( #6852, #13275, #12000, #11047, #9939, #6048, #6284, #2613, #8750, #15671, #227, #12235, #5087, #7393, #2293, #1336, #14715, #2456 ),
 .UNSPECIFIED., .F., .F.,
 ( 4, 2, 2, 2, 2, 2, 2, 2, 4 ),
 ( 0.000000000000000000, 0.0003914898357794977120, 0.0007829796715589954241, 0.001174469507338493082, 0.001565959343117990848, 0.001957449178897487096, 0.002348939014676983995, 0.002740428850456480461, 0.003131918686235977359 ),
 .UNSPECIFIED. ) ;
#306 = CARTESIAN_POINT ( 'NONE',  ( -5.842945980534678618, 1.369128644668824446, 4.126215691297385746 ) ) ;
#307 = FACE_OUTER_BOUND ( 'NONE', #5177, .T. ) ;
#308 = CARTESIAN_POINT ( 'NONE',  ( 3.735808404764892732, 4.696639218303211294, 17.02601979877759319 ) ) ;
#309 = CARTESIAN_POINT ( 'NONE',  ( 2.593621171579884699, 189.1921907459377792, 8.687688957072346341 ) ) ;
#310 = CARTESIAN_POINT ( 'NONE',  ( 0.03370811714257901381, -0.3999999999999941380, -2.527096502121718657 ) ) ;
#311 = CARTESIAN_POINT ( 'NONE',  ( 3.001999740804089711, 189.8855686313634124, 7.133436250992125416 ) ) ;
#312 = CARTESIAN_POINT ( 'NONE',  ( -0.9737725088280894115, -6.173885267451843184, 17.73735758726564882 ) ) ;
#313 = DIRECTION ( 'NONE',  ( 0.000000000000000000, 0.000000000000000000, -1.000000000000000000 ) ) ;
#314 = CARTESIAN_POINT ( 'NONE',  ( 0.8499999999999896527, -0.3999999999999906408, -2.750000000000010658 ) ) ;
#315 = ORIENTED_EDGE ( 'NONE', *, *, #1912, .F. ) ;
#316 = CARTESIAN_POINT ( 'NONE',  ( 0.8561741729129460632, 186.6999999989075150, 9.066987299999999195 ) ) ;
#317 =( BOUNDED_CURVE ( )  B_SPLINE_CURVE ( 2, ( #9057, #7531, #11422, #13807, #6512 ),
 .UNSPECIFIED., .F., .F. ) 
 B_SPLINE_CURVE_WITH_KNOTS ( ( 3, 2, 3 ),
 ( 0.8571428571428570953, 0.8750000000000000000, 0.8928571428571429047 ),
 .UNSPECIFIED. ) 
 CURVE ( )  GEOMETRIC_REPRESENTATION_ITEM ( )  RATIONAL_B_SPLINE_CURVE ( ( 1.000000000000000000, 0.9238795325112867385, 1.000000000000000000, 0.9238795325112867385, 1.000000000000000000 ) ) 
 REPRESENTATION_ITEM ( '' )  );
#318 = EDGE_LOOP ( 'NONE', ( #11239, #13450, #15608, #14902 ) ) ;
#319 = DIRECTION ( 'NONE',  ( 1.000000000000000000, 0.000000000000000000, 0.000000000000000000 ) ) ;
#320 = VERTEX_POINT ( 'NONE', #684 ) ;
#321 = CIRCLE ( 'NONE', #9221, 2.649388036945190095 ) ;
#322 = CARTESIAN_POINT ( 'NONE',  ( -5.915653884842670962, -1.003805156977642943, 25.00439760644211518 ) ) ;
#323 = SURFACE_STYLE_FILL_AREA ( #10269 ) ;
#324 = ORIENTED_EDGE ( 'NONE', *, *, #12407, .T. ) ;
#325 = CARTESIAN_POINT ( 'NONE',  ( -2.066987299999999639, 0.8561741729129452860, 0.4000000010924749105 ) ) ;
#326 = CARTESIAN_POINT ( 'NONE',  ( -1.767766952966369098, 1.767766952966369098, -1.600000000000000311 ) ) ;
#327 = CARTESIAN_POINT ( 'NONE',  ( -2.997549271363485701, 189.8887934741522088, 7.062685571753808844 ) ) ;
#328 = CARTESIAN_POINT ( 'NONE',  ( -5.940390500375766436, 6.474944468551470322, 17.99999999999998934 ) ) ;
#329 = CARTESIAN_POINT ( 'NONE',  ( -2.500000000000000444, 1.035533905932737753, 0.05000000000000014155 ) ) ;
#330 =( BOUNDED_CURVE ( )  B_SPLINE_CURVE ( 2, ( #15027, #7780, #6448, #7628, #12471, #4120, #1572, #12627, #6600 ),
 .UNSPECIFIED., .F., .F. ) 
 B_SPLINE_CURVE_WITH_KNOTS ( ( 3, 2, 2, 2, 3 ),
 ( 0.3571428571428572063, 0.3750000000000000555, 0.3928571428571429047, 0.4107142857142856984, 0.4285714285714285476 ),
 .UNSPECIFIED. ) 
 CURVE ( )  GEOMETRIC_REPRESENTATION_ITEM ( )  RATIONAL_B_SPLINE_CURVE ( ( 0.9999999999999997780, 0.9238795325112869605, 1.000000000000000000, 0.9238795325112867385, 1.000000000000000000, 0.9238795325112867385, 1.000000000000000000, 0.9238795325112867385, 1.000000000000000000 ) ) 
 REPRESENTATION_ITEM ( '' )  );
#331 = CARTESIAN_POINT ( 'NONE',  ( -4.005361199354992685, -4.468319061418773330, 10.69977782616119022 ) ) ;
#332 = CARTESIAN_POINT ( 'NONE',  ( 2.692143549875401831, 5.362363179736477470, 5.261943240031468960 ) ) ;
#333 = CARTESIAN_POINT ( 'NONE',  ( 0.8561741729129451750, 2.066987299999999639, -1.199999998907525622 ) ) ;
#334 = CARTESIAN_POINT ( 'NONE',  ( 5.616116467183661420, -2.743044348085539319, 10.99574050496990019 ) ) ;
#335 = CARTESIAN_POINT ( 'NONE',  ( -0.9735954530125078277, 6.173909381473996483, 31.26281793585242852 ) ) ;
#336 = ORIENTED_EDGE ( 'NONE', *, *, #9119, .T. ) ;
#337 = ORIENTED_EDGE ( 'NONE', *, *, #6167, .T. ) ;
#338 = VERTEX_POINT ( 'NONE', #15412 ) ;
#339 = CARTESIAN_POINT ( 'NONE',  ( 0.2638277032950181455, 5.995407492418034501, 18.97332055281517427 ) ) ;
#340 = CARTESIAN_POINT ( 'NONE',  ( 1.414552619335309291, 189.0000000000000853, 9.066428886377552843 ) ) ;
#341 = ORIENTED_EDGE ( 'NONE', *, *, #869, .F. ) ;
#342 = DIRECTION ( 'NONE',  ( 0.000000000000000000, -2.775557561562887900E-16, 1.000000000000000000 ) ) ;
#343 = AXIS2_PLACEMENT_3D ( 'NONE', #14019, #15537, #15300 ) ;
#344 = CARTESIAN_POINT ( 'NONE',  ( 0.8002302970946665317, -5.947135855825865569, 30.38601773212297985 ) ) ;
#345 = CARTESIAN_POINT ( 'NONE',  ( -3.255128505894313573, 5.336774832660720058, 31.87380055247395561 ) ) ;
#346 = CARTESIAN_POINT ( 'NONE',  ( 0.5030929395821815975, 6.230885867001134670, 17.12600319116549841 ) ) ;
#347 = CARTESIAN_POINT ( 'NONE',  ( -1.035533905932737753, 184.9499999978150413, 4.500000000000000888 ) ) ;
#348 = CARTESIAN_POINT ( 'NONE',  ( 5.131373506000546314, 7.062729720844130199, 11.49999999999998224 ) ) ;
#349 = CARTESIAN_POINT ( 'NONE',  ( 5.665824935993635236, -1.978765057080846601, 12.49995053646221166 ) ) ;
#350 = CARTESIAN_POINT ( 'NONE',  ( -3.882673863916385137, 4.899192824800864265, 18.97408542334169823 ) ) ;
#351 = DIRECTION ( 'NONE',  ( 0.000000000000000000, -1.000000000000000000, 0.000000000000000000 ) ) ;
#352 = CARTESIAN_POINT ( 'NONE',  ( 2.500000000000000444, 187.1199999975965795, 8.035533905932739529 ) ) ;
#353 = CARTESIAN_POINT ( 'NONE',  ( -1.885954199498669270, 228.0508284750123664, 6.386186391668034368 ) ) ;
#354 = CARTESIAN_POINT ( 'NONE',  ( -2.087773716237738331, 226.5967140655768048, 5.287030890998575927 ) ) ;
#355 = EDGE_CURVE ( 'NONE', #9607, #3437, #6727, .T. ) ;
#356 = CARTESIAN_POINT ( 'NONE',  ( -2.971600176645282421, 189.3276089958123976, 6.470516599052638540 ) ) ;
#357 = ORIENTED_EDGE ( 'NONE', *, *, #9015, .F. ) ;
#358 = EDGE_CURVE ( 'NONE', #3603, #7463, #3951, .T. ) ;
#359 = CARTESIAN_POINT ( 'NONE',  ( -6.176542424588100211, 0.9554180641286806885, 17.86762589283693359 ) ) ;
#360 = CARTESIAN_POINT ( 'NONE',  ( -2.500000000000000000, 0.000000000000000000, 1.700000000000000178 ) ) ;
#361 = CARTESIAN_POINT ( 'NONE',  ( -0.7993401192311853087, 6.199366368793661763, 5.614832469365748757 ) ) ;
#362 = CARTESIAN_POINT ( 'NONE',  ( 5.903472034603497676, 2.056448723545192259, 12.50008219321554570 ) ) ;
#363 = CARTESIAN_POINT ( 'NONE',  ( 2.825502441289275968, 227.6141739403474844, 8.283116510204369121 ) ) ;
#364 = EDGE_CURVE ( 'NONE', #4594, #6555, #9214, .T. ) ;
#365 = CARTESIAN_POINT ( 'NONE',  ( 2.848235266350880757, -5.281699484015723201, 23.88602261056919218 ) ) ;
#366 = CARTESIAN_POINT ( 'NONE',  ( -1.265664690411614835E-16, 2.066987299999999639, -1.149999998907525356 ) ) ;
#367 = CARTESIAN_POINT ( 'NONE',  ( 5.935543223013858061, -0.8771126767606637342, 4.869383044678627925 ) ) ;
#368 = CARTESIAN_POINT ( 'NONE',  ( -4.416837305303453753, -4.422286678979054919, 30.73809786915987630 ) ) ;
#369 = CARTESIAN_POINT ( 'NONE',  ( -2.500000000000000444, 185.1500000000000057, 5.964466094067261359 ) ) ;
#370 = FACE_BOUND ( 'NONE', #9710, .T. ) ;
#371 = CARTESIAN_POINT ( 'NONE',  ( -1.786743523428754976, 227.9724114945277051, 6.159713679416685572 ) ) ;
#372 = CARTESIAN_POINT ( 'NONE',  ( 2.066987300000000083, -0.8561741729129450640, -1.399999998907525134 ) ) ;
#373 = CARTESIAN_POINT ( 'NONE',  ( 2.500000000000000000, 3.061616997868383141E-16, -2.599999997815050534 ) ) ;
#374 = CARTESIAN_POINT ( 'NONE',  ( 0.8561741729129452860, 2.066987299999999639, 1.800000001092475044 ) ) ;
#375 = CARTESIAN_POINT ( 'NONE',  ( -1.767766952966369542, 184.5000000000000000, 8.767766952966368876 ) ) ;
#376 = CARTESIAN_POINT ( 'NONE',  ( -5.866984344570811416, -1.259800266528728008, 18.79931806258173665 ) ) ;
#378 = ORIENTED_EDGE ( 'NONE', *, *, #15661, .F. ) ;
#377 = CARTESIAN_POINT ( 'NONE',  ( -2.066987300000000083, 186.4499999989075150, 7.000000000000000000 ) ) ;
#379 = CARTESIAN_POINT ( 'NONE',  ( 2.500000000000000000, 3.061616997868383141E-16, -0.2999999999999999334 ) ) ;
#380 = CARTESIAN_POINT ( 'NONE',  ( 0.000000000000000000, 184.0000000000000000, 7.000000000000000000 ) ) ;
#381 = CARTESIAN_POINT ( 'NONE',  ( -5.999999999999999112, 227.2817795252328210, 4.165129161027028459 ) ) ;
#382 = CARTESIAN_POINT ( 'NONE',  ( 3.922396193918944896, 4.541970110199535782, 17.12619317285288645 ) ) ;
#383 = CARTESIAN_POINT ( 'NONE',  ( 1.818048556411949068, 189.7463703733489524, 9.770364204685183296 ) ) ;
#384 = CARTESIAN_POINT ( 'NONE',  ( 0.06404007393981200891, -0.3999999999999941380, -2.546123937053038855 ) ) ;
#385 = CARTESIAN_POINT ( 'NONE',  ( 2.692335458626972766, -5.362264153667172906, 5.262398918055980701 ) ) ;
#386 = CARTESIAN_POINT ( 'NONE',  ( -3.923477796648569882, 4.541042560386435945, 30.12696220972948780 ) ) ;
#387 = CARTESIAN_POINT ( 'NONE',  ( 0.2023276174656383763, -0.3999999999999898637, 2.561683098399103020 ) ) ;
#388 = CARTESIAN_POINT ( 'NONE',  ( -0.8070991676978370721, 189.0000000000000000, 4.628151146390497850 ) ) ;
#389 = ORIENTED_EDGE ( 'NONE', *, *, #6341, .F. ) ;
#390 = CARTESIAN_POINT ( 'NONE',  ( -1.461580736456473240, 185.7499999989074979, 8.461580736456472351 ) ) ;
#391 = AXIS2_PLACEMENT_3D ( 'NONE', #8568, #1379, #7592 ) ;
#392 = ORIENTED_EDGE ( 'NONE', *, *, #2098, .F. ) ;
#393 = DIRECTION ( 'NONE',  ( 1.000000000000000000, 0.000000000000000000, 0.000000000000000000 ) ) ;
#394 = ORIENTED_EDGE ( 'NONE', *, *, #3851, .T. ) ;
#395 = ADVANCED_FACE ( 'NONE', ( #5557 ), #9444, .F. ) ;
#396 = CARTESIAN_POINT ( 'NONE',  ( 2.082642335314403343E-14, -6.250000000000000888, 31.00000000000000000 ) ) ;
#397 = CYLINDRICAL_SURFACE ( 'NONE', #7859, 1.000000000000000888 ) ;
#398 = VERTEX_POINT ( 'NONE', #14205 ) ;
#399 = CARTESIAN_POINT ( 'NONE',  ( 2.066987299999999639, 0.8561741729129456191, -2.299999998907525711 ) ) ;
#400 = CARTESIAN_POINT ( 'NONE',  ( -4.290821322214388722, 4.545321419741542357, 4.385580527545153373 ) ) ;
#401 = CARTESIAN_POINT ( 'NONE',  ( -0.3832019641432907187, 228.2493259063060691, 10.15123907897345568 ) ) ;
#402 = DIRECTION ( 'NONE',  ( 1.000000000000000000, 0.000000000000000000, 0.000000000000000000 ) ) ;
#403 = CARTESIAN_POINT ( 'NONE',  ( -2.500000000000000000, 0.000000000000000000, 1.800000002184949821 ) ) ;
#404 = CARTESIAN_POINT ( 'NONE',  ( -5.984595133899170527, -1.806709459528687667, 5.999950789842938725 ) ) ;
#405 = CARTESIAN_POINT ( 'NONE',  ( -2.849269941561969333, -5.281123252784043487, 10.88480617551147667 ) ) ;
#406 = CARTESIAN_POINT ( 'NONE',  ( 1.035533905932737531, 2.500000000000000444, -0.8499999978150500901 ) ) ;
#407 = CARTESIAN_POINT ( 'NONE',  ( 3.796994071234844259E-16, -2.066987299999999639, 0.05000000109247476621 ) ) ;
#408 =( BOUNDED_CURVE ( )  B_SPLINE_CURVE ( 2, ( #13845, #5357, #15207, #15052, #7888, #406, #8045, #8938, #10125 ),
 .UNSPECIFIED., .F., .F. ) 
 B_SPLINE_CURVE_WITH_KNOTS ( ( 3, 2, 2, 2, 3 ),
 ( 0.4285714285714285476, 0.4464285714285714524, 0.4642857142857143016, 0.4821428571428571508, 0.5000000000000000000 ),
 .UNSPECIFIED. ) 
 CURVE ( )  GEOMETRIC_REPRESENTATION_ITEM ( )  RATIONAL_B_SPLINE_CURVE ( ( 1.000000000000000000, 0.9238795325112867385, 1.000000000000000000, 0.9238795325112867385, 1.000000000000000000, 0.9238795325112867385, 1.000000000000000000, 0.9238795325112867385, 1.000000000000000000 ) ) 
 REPRESENTATION_ITEM ( '' )  );
#409 = DIRECTION ( 'NONE',  ( 1.000000000000000000, 0.000000000000000000, 0.000000000000000000 ) ) ;
#410 = CARTESIAN_POINT ( 'NONE',  ( 2.500000000000000444, 186.3499999978150754, 5.964466094067262247 ) ) ;
#411 = ORIENTED_EDGE ( 'NONE', *, *, #6538, .F. ) ;
#412 = EDGE_LOOP ( 'NONE', ( #8229, #15228, #15119, #15116 ) ) ;
#413 = VECTOR ( 'NONE', #15523, 1000.000000000000000 ) ;
#414 = ORIENTED_EDGE ( 'NONE', *, *, #5071, .T. ) ;
#415 = CARTESIAN_POINT ( 'NONE',  ( 0.7988914244719601543, 5.947301735519265442, 17.38456289168617985 ) ) ;
#416 = CARTESIAN_POINT ( 'NONE',  ( 1.644293607015084646, 189.0000000000000568, 8.888752495498886574 ) ) ;
#417 = ORIENTED_EDGE ( 'NONE', *, *, #12558, .T. ) ;
#418 = CARTESIAN_POINT ( 'NONE',  ( -0.5031281619707669295, -5.980084330432671180, 4.126022727445256777 ) ) ;
#419 = CARTESIAN_POINT ( 'NONE',  ( -6.176542424588117974, 0.9554180641285661135, 31.00000000000000000 ) ) ;
#420 = CARTESIAN_POINT ( 'NONE',  ( -0.5039005892419784471, 6.230833003620553256, 17.12636388911295526 ) ) ;
#421 = CARTESIAN_POINT ( 'NONE',  ( 0.2623718222036656722, 6.245654667075778654, 17.02627829713834373 ) ) ;
#422 = CARTESIAN_POINT ( 'NONE',  ( -1.035533905932737975, 186.5499999978150640, 4.500000000000000888 ) ) ;
#423 = CARTESIAN_POINT ( 'NONE',  ( 2.500000000000000444, 184.7499999978150527, 5.964466094067262247 ) ) ;
#424 = AXIS2_PLACEMENT_3D ( 'NONE', #6276, #8742, #11195 ) ;
#425 = CARTESIAN_POINT ( 'NONE',  ( 5.935543223013868719, 0.8771126767606117758, 18.13061695532137563 ) ) ;
#426 = DIRECTION ( 'NONE',  ( 0.000000000000000000, -1.000000000000000000, 0.000000000000000000 ) ) ;
#427 = CARTESIAN_POINT ( 'NONE',  ( -1.767766952966369765, 187.6699999975965625, 8.767766952966368876 ) ) ;
#428 = CARTESIAN_POINT ( 'NONE',  ( 0.6320692372082544752, 228.2335842258707430, 10.10492066627648988 ) ) ;
#429 = CARTESIAN_POINT ( 'NONE',  ( -2.980755195990519191, 227.3998431049529074, 7.652341518474168325 ) ) ;
#430 = EDGE_LOOP ( 'NONE', ( #165, #8727 ) ) ;
#431 = CARTESIAN_POINT ( 'NONE',  ( -2.464020019946891793, 189.7914691120035400, 9.078875626642586738 ) ) ;
#432 = ORIENTED_EDGE ( 'NONE', *, *, #11524, .T. ) ;
#433 = CARTESIAN_POINT ( 'NONE',  ( -5.615973259022290165, 2.743340227996234226, 17.49610786875029689 ) ) ;
#434 = CARTESIAN_POINT ( 'NONE',  ( -6.142908455506919552, 1.155755562476170839, 23.88482219624156855 ) ) ;
#435 = DIRECTION ( 'NONE',  ( 0.000000000000000000, 0.000000000000000000, -1.000000000000000000 ) ) ;
#436 = CARTESIAN_POINT ( 'NONE',  ( 5.571002711501404470, 2.833546409886289030, 11.76379616840804232 ) ) ;
#437 = CARTESIAN_POINT ( 'NONE',  ( 2.938271602351877121, 227.0923189680254666, 6.746872328837914878 ) ) ;
#438 = CARTESIAN_POINT ( 'NONE',  ( 2.840966774240223369, 5.567223638426877841, 5.261902130840121039 ) ) ;
#439 = CARTESIAN_POINT ( 'NONE',  ( 1.035533905932737531, 2.500000000000000444, 1.450000000000000400 ) ) ;
#440 = LINE ( 'NONE', #9200, #5916 ) ;
#441 = CARTESIAN_POINT ( 'NONE',  ( 0.000000000000000000, -0.3999999999999958589, -2.450963827680254337 ) ) ;
#442 = B_SPLINE_CURVE_WITH_KNOTS ( 'NONE', 3,
 ( #14232, #2140, #3189, #9317, #15286, #5742, #4389, #1910, #5509, #9242, #12806, #718, #1989, #8126, #11536, #6706, #14078, #6862 ),
 .UNSPECIFIED., .F., .F.,
 ( 4, 2, 2, 2, 2, 2, 2, 2, 4 ),
 ( 0.003131918686235976492, 0.003523310662250267195, 0.003914702638264558332, 0.004306094614278849035, 0.004697486590293139738, 0.005088878566307430441, 0.005480270542321721144, 0.005871662518336011848, 0.006263054494350302551 ),
 .UNSPECIFIED. ) ;
#443 = DIRECTION ( 'NONE',  ( 0.000000000000000000, 1.000000000000000000, 0.000000000000000000 ) ) ;
#444 = CARTESIAN_POINT ( 'NONE',  ( -1.035533905932739751, 186.9499999999999886, 9.500000000000003553 ) ) ;
#445 = EDGE_CURVE ( 'NONE', #2248, #14335, #14582, .T. ) ;
#446 = AXIS2_PLACEMENT_3D ( 'NONE', #11551, #13858, #6488 ) ;
#447 = CARTESIAN_POINT ( 'NONE',  ( -1.385362557672197736, 227.7924883072852822, 5.640085252515396164 ) ) ;
#448 = CARTESIAN_POINT ( 'NONE',  ( 5.000000000000000000, 6.123233995736765296E-16, 52.97056274847714263 ) ) ;
#449 = CARTESIAN_POINT ( 'NONE',  ( -2.997451966578398075, -5.485105005466015982, 10.88482219624155967 ) ) ;
#450 = LINE ( 'NONE', #2848, #4783 ) ;
#451 = CARTESIAN_POINT ( 'NONE',  ( -1.456896669277396583E-16, 188.4499999989075150, 4.933012699999999029 ) ) ;
#452 = CARTESIAN_POINT ( 'NONE',  ( -2.782713018890758061, 5.315928322779098991, 18.50439760644211518 ) ) ;
#454 = ORIENTED_EDGE ( 'NONE', *, *, #12708, .F. ) ;
#453 = CARTESIAN_POINT ( 'NONE',  ( -2.066987300000000527, 188.7999999989075093, 6.143825827087054492 ) ) ;
#455 = CARTESIAN_POINT ( 'NONE',  ( -2.841041022017427142, -5.567186575787240521, 17.73774718278285434 ) ) ;
#457 = EDGE_CURVE ( 'NONE', #15709, #6637, #10482, .T. ) ;
#456 = VECTOR ( 'NONE', #13750, 1000.000000000000000 ) ;
#458 = FACE_OUTER_BOUND ( 'NONE', #7735, .T. ) ;
#459 = CARTESIAN_POINT ( 'NONE',  ( 0.7081379353438700397, 0.4000000000000047962, -2.606463079733443600 ) ) ;
#460 = EDGE_CURVE ( 'NONE', #3041, #9290, #14361, .T. ) ;
#461 = CARTESIAN_POINT ( 'NONE',  ( 2.837060236510290157, 189.8314984584918079, 8.326472016722609837 ) ) ;
#462 = DIRECTION ( 'NONE',  ( 0.5877852522924802425, -0.8090169943749422332, 0.000000000000000000 ) ) ;
#463 = CARTESIAN_POINT ( 'NONE',  ( -5.935543223013843850, -0.8771126767607685393, 31.00000000000000000 ) ) ;
#465 = CYLINDRICAL_SURFACE ( 'NONE', #13069, 1.000000000000000222 ) ;
#464 = AXIS2_PLACEMENT_3D ( 'NONE', #9917, #5307, #2906 ) ;
#466 = CARTESIAN_POINT ( 'NONE',  ( 0.000000000000000000, 184.0000000000000000, 0.000000000000000000 ) ) ;
#467 = VECTOR ( 'NONE', #1666, 1000.000000000000000 ) ;
#468 = CARTESIAN_POINT ( 'NONE',  ( -5.620879908643933831, -2.102487719021981949, 10.52622176056705428 ) ) ;
#469 = ORIENTED_EDGE ( 'NONE', *, *, #9305, .F. ) ;
#470 = CARTESIAN_POINT ( 'NONE',  ( -2.066987300000000971, 187.9999999989075263, 6.143825827087054492 ) ) ;
#471 = VERTEX_POINT ( 'NONE', #4671 ) ;
#472 = CARTESIAN_POINT ( 'NONE',  ( -5.915641100987803824, 1.003868594704913519, 25.00428920362019625 ) ) ;
#473 = ORIENTED_EDGE ( 'NONE', *, *, #2610, .T. ) ;
#474 = EDGE_CURVE ( 'NONE', #3929, #6460, #15716, .T. ) ;
#475 = CYLINDRICAL_SURFACE ( 'NONE', #10388, 1.000000000000000666 ) ;
#476 = DIRECTION ( 'NONE',  ( 0.000000000000000000, 0.000000000000000000, 1.000000000000000000 ) ) ;
#477 = APPLICATION_CONTEXT ( 'automotive_design' ) ;
#478 = VERTEX_POINT ( 'NONE', #125 ) ;
#479 = AXIS2_PLACEMENT_3D ( 'NONE', #15199, #7061, #4294 ) ;
#480 = CARTESIAN_POINT ( 'NONE',  ( 2.066987300000000083, -0.8561741729129449530, -2.399999998907525356 ) ) ;
#481 = DIRECTION ( 'NONE',  ( -6.123233995736766036E-17, 1.000000000000000000, 0.000000000000000000 ) ) ;
#482 = CARTESIAN_POINT ( 'NONE',  ( -9.750000000000003553, 3.401296724241641415E-14, 2.000000000000001776 ) ) ;
#483 = CARTESIAN_POINT ( 'NONE',  ( 1.767766952966369320, -1.767766952966368654, -0.4000000000000001887 ) ) ;
#484 = CARTESIAN_POINT ( 'NONE',  ( -6.176542424588106428, -0.9554180641286325049, 5.132374107163055754 ) ) ;
#485 = CARTESIAN_POINT ( 'NONE',  ( -4.286401442266578599, -4.198423832313146420, 11.49999999999998224 ) ) ;
#486 = DIRECTION ( 'NONE',  ( 0.000000000000000000, 0.000000000000000000, 1.000000000000000000 ) ) ;
#487 = CARTESIAN_POINT ( 'NONE',  ( -1.265664690411614835E-16, 2.066987299999999639, -1.149999998907525356 ) ) ;
#488 = EDGE_CURVE ( 'NONE', #14260, #5268, #1225, .T. ) ;
#489 = CARTESIAN_POINT ( 'NONE',  ( 4.142173849413700815, 4.341773579105447922, 12.11519382448850557 ) ) ;
#490 = ORIENTED_EDGE ( 'NONE', *, *, #8030, .T. ) ;
#491 = AXIS2_PLACEMENT_3D ( 'NONE', #7668, #1615, #14760 ) ;
#492 = PRODUCT_RELATED_PRODUCT_CATEGORY ( 'part', '', ( #6017 ) ) ;
#493 = ORIENTED_EDGE ( 'NONE', *, *, #9967, .T. ) ;
#494 = EDGE_CURVE ( 'NONE', #11779, #1022, #11976, .T. ) ;
#495 = ORIENTED_EDGE ( 'NONE', *, *, #4351, .F. ) ;
#496 = CARTESIAN_POINT ( 'NONE',  ( -6.176542424588095770, -0.9554180641287001174, 11.49999999999998224 ) ) ;
#497 = CARTESIAN_POINT ( 'NONE',  ( 5.903596343266263702, 2.055998103990681614, 4.000049210157071045 ) ) ;
#498 = EDGE_LOOP ( 'NONE', ( #13781, #14669 ) ) ;
#499 = CYLINDRICAL_SURFACE ( 'NONE', #8108, 1.500000000000001776 ) ;
#500 = CARTESIAN_POINT ( 'NONE',  ( 1.354942164390165777E-13, -6.250000000000000888, 16.99999999999998579 ) ) ;
#501 =( REPRESENTATION_RELATIONSHIP ('NONE','NONE', #11191, #4596 ) REPRESENTATION_RELATIONSHIP_WITH_TRANSFORMATION ( #7726 )SHAPE_REPRESENTATION_RELATIONSHIP( ) );
#502 = CARTESIAN_POINT ( 'NONE',  ( -5.330004929009617420, 2.755647751839342519, 5.262398918055979813 ) ) ;
#503 = CARTESIAN_POINT ( 'NONE',  ( 1.767766952966369320, -1.767766952966368654, -2.000000000000000444 ) ) ;
#504 = CARTESIAN_POINT ( 'NONE',  ( -2.500000000000000444, 185.0999999978150754, 7.000000000000000000 ) ) ;
#505 = CARTESIAN_POINT ( 'NONE',  ( 2.668367453516569121, 5.373994336898161528, 11.36938304467859773 ) ) ;
#506 = CARTESIAN_POINT ( 'NONE',  ( 1.767766952966368654, 185.4699999975965454, 8.767766952966368876 ) ) ;
#507 = CARTESIAN_POINT ( 'NONE',  ( 0.4870669733929915424, 228.2428440931186628, 10.13214456346285708 ) ) ;
#508 = CARTESIAN_POINT ( 'NONE',  ( -0.3933619333212962643, 226.3329841201265253, 4.509674143907711041 ) ) ;
#509 = ORIENTED_EDGE ( 'NONE', *, *, #12250, .F. ) ;
#510 = CARTESIAN_POINT ( 'NONE',  ( -2.055837405312323174, -1.429616716009805888, -2.499172079278979997 ) ) ;
#511 = B_SPLINE_CURVE_WITH_KNOTS ( 'NONE', 3,
 ( #8242, #10938, #9758, #13397, #14433, #4661, #3454, #10855, #2341, #13243, #11014, #2259, #5933, #3375, #14601, #14346, #36, #7047 ),
 .UNSPECIFIED., .F., .F.,
 ( 4, 2, 2, 2, 2, 2, 2, 2, 4 ),
 ( 0.003131486019301990727, 0.003522824630466696565, 0.003914163241631402404, 0.004305501852796108676, 0.004696840463960814081, 0.005088179075125522088, 0.005479517686290229228, 0.005870856297454936368, 0.006262194908619643507 ),
 .UNSPECIFIED. ) ;
#512 = VERTEX_POINT ( 'NONE', #14445 ) ;
#513 = CARTESIAN_POINT ( 'NONE',  ( -4.070863287254244511, 4.743975846881662406, 17.12694108445698760 ) ) ;
#514 = DIRECTION ( 'NONE',  ( 0.9510565162951499785, 0.3090169943749582204, 0.000000000000000000 ) ) ;
#515 = CARTESIAN_POINT ( 'NONE',  ( -0.1306394121199367930, 6.250000000000000888, 4.000000000000004441 ) ) ;
#516 = CARTESIAN_POINT ( 'NONE',  ( 5.903596343266268143, 2.055998103990667403, 30.00004921015706572 ) ) ;
#517 = CARTESIAN_POINT ( 'NONE',  ( 2.959395828221181191, 227.1267441636075262, 6.848257790201431661 ) ) ;
#518 = CARTESIAN_POINT ( 'NONE',  ( 4.142173849413673281, -4.341773579105472791, 23.88480617551147844 ) ) ;
#519 = CARTESIAN_POINT ( 'NONE',  ( 1.461580736456472573, 1.461580736456472795, -1.249999998907525223 ) ) ;
#520 = CARTESIAN_POINT ( 'NONE',  ( -4.267838854167106177, -4.217593933790406702, 31.26239891805596827 ) ) ;
#521 = PRESENTATION_STYLE_ASSIGNMENT (( #13881 ) ) ;
#522 = CARTESIAN_POINT ( 'NONE',  ( -5.131373506000878493, 7.062729720843910819, 24.49999999999999289 ) ) ;
#523 = CARTESIAN_POINT ( 'NONE',  ( -5.929230630780102373E-16, 186.2000000000000171, 9.500000000000001776 ) ) ;
#524 = EDGE_CURVE ( 'NONE', #8787, #10326, #14889, .T. ) ;
#525 = CARTESIAN_POINT ( 'NONE',  ( -1.313542798833678749, 227.7708088449086290, 5.577473728656160645 ) ) ;
#526 = PRODUCT_DEFINITION_CONTEXT ( 'detailed design', #5064, 'design' ) ;
#527 = FACE_BOUND ( 'NONE', #5862, .T. ) ;
#528 = CARTESIAN_POINT ( 'NONE',  ( -0.8561741729129458411, -2.066987299999999195, -1.799999998907525045 ) ) ;
#529 = CARTESIAN_POINT ( 'NONE',  ( -2.500000000000000444, 185.2000000000000171, 7.000000000000000000 ) ) ;
#530 = CARTESIAN_POINT ( 'NONE',  ( -5.915653884842685173, -1.003805156977577662, 18.50439760644211518 ) ) ;
#532 = ORIENTED_EDGE ( 'NONE', *, *, #10481, .F. ) ;
#531 = CARTESIAN_POINT ( 'NONE',  ( 2.066987300000000083, 186.8999999989075320, 6.143825827087054492 ) ) ;
#533 = VECTOR ( 'NONE', #5560, 1000.000000000000000 ) ;
#534 = EDGE_CURVE ( 'NONE', #7505, #3363, #14632, .T. ) ;
#535 = CARTESIAN_POINT ( 'NONE',  ( -4.286401442266626560, -4.198423832313095794, 17.86935038651143515 ) ) ;
#536 = CARTESIAN_POINT ( 'NONE',  ( 5.935543223013878489, -0.8771126767605277319, 17.86938304467860306 ) ) ;
#537 = CARTESIAN_POINT ( 'NONE',  ( 0.03982005317027621089, 190.0874997052910658, 4.201869497416318211 ) ) ;
#538 =( LENGTH_UNIT ( ) NAMED_UNIT ( * ) SI_UNIT ( .MILLI., .METRE. ) );
#539 = CARTESIAN_POINT ( 'NONE',  ( 3.012851251850296563, 189.2892816699357468, 7.217589605582900525 ) ) ;
#540 = CARTESIAN_POINT ( 'NONE',  ( 0.009591240409140278089, -0.3999999999999975797, -2.494254166949156026 ) ) ;
#541 = CARTESIAN_POINT ( 'NONE',  ( -0.6139908388540702422, 5.969238533166615568, 30.19977627912012252 ) ) ;
#542 = CARTESIAN_POINT ( 'NONE',  ( 1.582454879690585958, 190.0440573869416312, 4.656039093731057399 ) ) ;
#543 = LINE ( 'NONE', #1579, #12817 ) ;
#544 = CARTESIAN_POINT ( 'NONE',  ( -5.666074146197981776, -1.978051345703211839, 12.50004932073310471 ) ) ;
#545 = DIRECTION ( 'NONE',  ( -0.000000000000000000, 1.000000000000000000, -0.000000000000000000 ) ) ;
#546 = VERTEX_POINT ( 'NONE', #7374 ) ;
#547 = CARTESIAN_POINT ( 'NONE',  ( 0.8561741729129458411, 187.4999999989075548, 9.066987299999999195 ) ) ;
#548 = ORIENTED_EDGE ( 'NONE', *, *, #8965, .T. ) ;
#549 = CARTESIAN_POINT ( 'NONE',  ( -5.317509234263835260, -2.779225709351231366, 24.49999999999999289 ) ) ;
#550 = ADVANCED_FACE ( 'NONE', ( #2271 ), #7141, .T. ) ;
#551 = ORIENTED_EDGE ( 'NONE', *, *, #6800, .F. ) ;
#552 = DIRECTION ( 'NONE',  ( -6.123233995736766036E-17, 1.000000000000000000, 0.000000000000000000 ) ) ;
#553 = EDGE_CURVE ( 'NONE', #3385, #10225, #2858, .T. ) ;
#554 = FACE_OUTER_BOUND ( 'NONE', #8032, .T. ) ;
#555 = EDGE_LOOP ( 'NONE', ( #8215, #1137, #7408, #11561, #3893 ) ) ;
#556 = CARTESIAN_POINT ( 'NONE',  ( -3.000000000000000444, -1.732050807568878081, -5.500000000000000000 ) ) ;
#557 = EDGE_CURVE ( 'NONE', #1272, #898, #148, .T. ) ;
#558 = CARTESIAN_POINT ( 'NONE',  ( -0.5039079366031161689, 5.980031194523161453, 17.12637068109811977 ) ) ;
#559 = CARTESIAN_POINT ( 'NONE',  ( 5.317509234264064411, -2.779225709350791274, 24.49999999999999289 ) ) ;
#560 = CARTESIAN_POINT ( 'NONE',  ( -1.035533905932737753, 2.500000000000000444, -0.05000000000000014155 ) ) ;
#561 = DIRECTION ( 'NONE',  ( -0.000000000000000000, 1.000000000000000000, -0.000000000000000000 ) ) ;
#562 = PLANE ( 'NONE',  #12276 ) ;
#563 = CONTEXT_DEPENDENT_SHAPE_REPRESENTATION ( #7321, #7183 ) ;
#564 = DIRECTION ( 'NONE',  ( 0.000000000000000000, 0.000000000000000000, 1.000000000000000000 ) ) ;
#565 = CARTESIAN_POINT ( 'NONE',  ( -1.461580736456472795, 1.461580736456472795, -0.2499999989075251672 ) ) ;
#566 = CARTESIAN_POINT ( 'NONE',  ( 2.668367453516568677, 5.373994336898162416, 11.63064961348853465 ) ) ;
#567 = VERTEX_POINT ( 'NONE', #9606 ) ;
#568 = AXIS2_PLACEMENT_3D ( 'NONE', #14972, #12418, #11226 ) ;
#569 = ORIENTED_EDGE ( 'NONE', *, *, #5071, .F. ) ;
#570 = ORIENTED_EDGE ( 'NONE', *, *, #4975, .F. ) ;
#571 = CARTESIAN_POINT ( 'NONE',  ( -6.142844459177225325, -1.156093792145260979, 10.88439807107078394 ) ) ;
#572 = CARTESIAN_POINT ( 'NONE',  ( 6.155912734541117537, 1.081577393120979780, 4.496107868750329750 ) ) ;
#573 = ORIENTED_EDGE ( 'NONE', *, *, #355, .F. ) ;
#574 = CARTESIAN_POINT ( 'NONE',  ( 5.903347812666375205, -1.076697810262440491, 18.61397738943082203 ) ) ;
#575 = CARTESIAN_POINT ( 'NONE',  ( 1.035533905932739085, -2.500000000000000000, 0.4500000021849495657 ) ) ;
#576 = CARTESIAN_POINT ( 'NONE',  ( -0.9999505860952112579, 6.169489349035827352, 18.13105903165805799 ) ) ;
#577 = CARTESIAN_POINT ( 'NONE',  ( 5.859155363331400856, -2.178872204144929992, 30.02599901976670438 ) ) ;
#578 = CARTESIAN_POINT ( 'NONE',  ( 2.500000000000000444, 187.0499999978150640, 8.035533905932739529 ) ) ;
#579 = CIRCLE ( 'NONE', #3127, 2.500000000000000000 ) ;
#580 = LINE ( 'NONE', #4165, #11320 ) ;
#581 = CARTESIAN_POINT ( 'NONE',  ( 3.922396193918995522, 4.541970110199488708, 10.62619317285287934 ) ) ;
#582 = EDGE_CURVE ( 'NONE', #9339, #5163, #6425, .T. ) ;
#583 = CARTESIAN_POINT ( 'NONE',  ( 1.035533905932738197, 189.4199999975965625, 9.500000000000003553 ) ) ;
#584 = CARTESIAN_POINT ( 'NONE',  ( 2.379866841847371628, 227.8775224696199473, 9.057852156131547261 ) ) ;
#585 = CARTESIAN_POINT ( 'NONE',  ( -2.521794825564176890, 226.7667903661470348, 5.788166807254388146 ) ) ;
#586 = EDGE_CURVE ( 'NONE', #15318, #4525, #2806, .T. ) ;
#587 = EDGE_LOOP ( 'NONE', ( #4059, #13067, #6384, #6203 ) ) ;
#588 = CARTESIAN_POINT ( 'NONE',  ( 3.011899281037532461, -5.190111395030209351, 4.199777826161210648 ) ) ;
#589 = ORIENTED_EDGE ( 'NONE', *, *, #3180, .F. ) ;
#590 = CARTESIAN_POINT ( 'NONE',  ( 4.435347140101073116, -4.403429997944470209, 5.000000000000004441 ) ) ;
#591 = DIRECTION ( 'NONE',  ( -0.9510565162951545304, 0.3090169943749447867, 0.000000000000000000 ) ) ;
#592 = CARTESIAN_POINT ( 'NONE',  ( 1.461580736456473462, 184.3499999989074922, 5.538419263543526760 ) ) ;
#593 = CARTESIAN_POINT ( 'NONE',  ( -0.8737888311110042494, 5.936248257219510549, 5.503441851412170571 ) ) ;
#594 = EDGE_CURVE ( 'NONE', #12272, #12484, #3857, .T. ) ;
#595 = CARTESIAN_POINT ( 'NONE',  ( 3.882809187878910606, 4.899079348630070108, 10.52599901976669017 ) ) ;
#596 = CARTESIAN_POINT ( 'NONE',  ( 4.069684453406305025, 4.744965295353549273, 5.873800552473966263 ) ) ;
#597 = CARTESIAN_POINT ( 'NONE',  ( 6.143143148203058956, -1.154591847827712403, 31.61396179408071916 ) ) ;
#598 = CARTESIAN_POINT ( 'NONE',  ( -2.500000000000000000, -1.035533905932739307, -0.6500000000000000222 ) ) ;
#599 = CARTESIAN_POINT ( 'NONE',  ( 2.500000000000000000, 188.7999999999999829, 7.000000000000000000 ) ) ;
#600 = CARTESIAN_POINT ( 'NONE',  ( 5.935543223013847403, 0.8771126767607483332, 5.130616955321390726 ) ) ;
#601 = CARTESIAN_POINT ( 'NONE',  ( 2.500000000000000444, 186.4000000000000057, 7.000000000000000000 ) ) ;
#602 = CARTESIAN_POINT ( 'NONE',  ( -1.938951794131667850, 228.1124887269953092, 6.564264716264994526 ) ) ;
#603 = DIRECTION ( 'NONE',  ( 0.000000000000000000, 1.000000000000000000, 0.000000000000000000 ) ) ;
#604 = CARTESIAN_POINT ( 'NONE',  ( 6.172614129015239648, -0.9817721000788448560, 30.73763026556126832 ) ) ;
#605 = CARTESIAN_POINT ( 'NONE',  ( 2.066987299999999639, 2.531329380823229670E-16, -1.549999998907525489 ) ) ;
#606 = CARTESIAN_POINT ( 'NONE',  ( -2.500000000000000444, 188.3499999999999943, 5.964466094067261359 ) ) ;
#607 = FACE_OUTER_BOUND ( 'NONE', #2207, .T. ) ;
#609 = ORIENTED_EDGE ( 'NONE', *, *, #9405, .F. ) ;
#608 = CARTESIAN_POINT ( 'NONE',  ( -2.066987300000000527, 187.2999999989075661, 7.856174172912944620 ) ) ;
#610 = CARTESIAN_POINT ( 'NONE',  ( -3.922672396097112824, -4.541739265057652020, 17.12635295315576300 ) ) ;
#611 = CARTESIAN_POINT ( 'NONE',  ( 2.500000000000000444, 186.2999999978150356, 7.000000000000000000 ) ) ;
#612 = VECTOR ( 'NONE', #7149, 1000.000000000000000 ) ;
#613 = CARTESIAN_POINT ( 'NONE',  ( -5.487348639458814681, 2.428538342494583890, 23.69977782616121331 ) ) ;
#614 = PRESENTATION_STYLE_ASSIGNMENT (( #15259 ) ) ;
#615 = CARTESIAN_POINT ( 'NONE',  ( 1.855150134049648347, 188.9999999974870946, 5.314312548248043555 ) ) ;
#616 = LINE ( 'NONE', #4206, #9107 ) ;
#617 = CARTESIAN_POINT ( 'NONE',  ( -0.5039079366032207519, 5.980031194523153459, 30.12637068109813043 ) ) ;
#618 = CARTESIAN_POINT ( 'NONE',  ( 1.579185070784824285, 228.6572036374857078, 8.137432446265082220 ) ) ;
#619 = CARTESIAN_POINT ( 'NONE',  ( -4.286401442266607020, 4.198423832313117110, 31.00000000000000000 ) ) ;
#620 = CARTESIAN_POINT ( 'NONE',  ( -6.176542424588121527, 0.9554180641285457964, 4.867625892836954904 ) ) ;
#621 = DIRECTION ( 'NONE',  ( 0.9510565162951499785, 0.3090169943749582204, 0.000000000000000000 ) ) ;
#622 = ORIENTED_EDGE ( 'NONE', *, *, #10760, .T. ) ;
#623 = CARTESIAN_POINT ( 'NONE',  ( 0.8561741729129461742, 186.4999999989075263, 9.066987300000000971 ) ) ;
#624 = CARTESIAN_POINT ( 'NONE',  ( 2.668367453516611754, 5.373994336898140212, 30.86938304467861727 ) ) ;
#625 = ORIENTED_EDGE ( 'NONE', *, *, #13568, .F. ) ;
#626 = CYLINDRICAL_SURFACE ( 'NONE', #9896, 1.000000000000000888 ) ;
#627 = CARTESIAN_POINT ( 'NONE',  ( 2.500000000000000444, 185.5999999999999943, 7.000000000000000000 ) ) ;
#628 = CARTESIAN_POINT ( 'NONE',  ( -5.931734679891443207, -0.9039278060244418933, 30.73617396794404044 ) ) ;
#629 = CARTESIAN_POINT ( 'NONE',  ( -4.344762547369716899, 4.493114738039211353, 4.496913561339538568 ) ) ;
#630 = CARTESIAN_POINT ( 'NONE',  ( 2.066987300000000527, 184.2499999989074979, 7.000000000000000000 ) ) ;
#631 = DIRECTION ( 'NONE',  ( -0.8660254037844387076, -0.4999999999999998890, 0.000000000000000000 ) ) ;
#632 = CARTESIAN_POINT ( 'NONE',  ( 1.035533905932737531, 2.500000000000000444, -1.750000000000000222 ) ) ;
#633 = DIRECTION ( 'NONE',  ( 0.000000000000000000, 0.000000000000000000, 1.000000000000000000 ) ) ;
#634 = CARTESIAN_POINT ( 'NONE',  ( -4.196038884587174778, -4.289036423669268849, 10.99610204984015205 ) ) ;
#635 = EDGE_CURVE ( 'NONE', #13364, #1681, #12596, .T. ) ;
#636 = DIRECTION ( 'NONE',  ( -0.9510565162951545304, 0.3090169943749447867, 0.000000000000000000 ) ) ;
#637 = CARTESIAN_POINT ( 'NONE',  ( 4.344313232727101237, 4.493553492990120191, 31.50436969680151833 ) ) ;
#638 = CARTESIAN_POINT ( 'NONE',  ( 6.000000000000000000, 7.347880794884118750E-16, 36.00000000000000711 ) ) ;
#639 = EDGE_CURVE ( 'NONE', #1178, #15136, #14644, .T. ) ;
#640 = EDGE_LOOP ( 'NONE', ( #3910, #10945 ) ) ;
#641 = ORIENTED_EDGE ( 'NONE', *, *, #11646, .T. ) ;
#642 = VERTEX_POINT ( 'NONE', #5309 ) ;
#643 = CARTESIAN_POINT ( 'NONE',  ( 3.010624175977885120, -5.190832888732274775, 25.29888242247941221 ) ) ;
#644 = DIRECTION ( 'NONE',  ( 0.000000000000000000, 0.000000000000000000, 1.000000000000000000 ) ) ;
#645 = VERTEX_POINT ( 'NONE', #6427 ) ;
#646 = CARTESIAN_POINT ( 'NONE',  ( 4.592425496802573972E-16, -2.500000000000000000, 0.4000000021849496878 ) ) ;
#647 = CARTESIAN_POINT ( 'NONE',  ( -1.000049271338347534, 6.169473353325575005, 17.86969612704546506 ) ) ;
#648 = CARTESIAN_POINT ( 'NONE',  ( -2.997451966578351001, -5.485105005466042627, 4.384822196241565884 ) ) ;
#649 = CARTESIAN_POINT ( 'NONE',  ( -0.8561741729129466183, 184.9999999989074979, 9.066987299999999195 ) ) ;
#650 = CARTESIAN_POINT ( 'NONE',  ( -9.148167235839370302E-31, 189.0000000000000000, 4.500000000000000888 ) ) ;
#651 = CARTESIAN_POINT ( 'NONE',  ( -6.176542424588088664, 0.9554180641287480791, 24.49999999999999289 ) ) ;
#652 = EDGE_CURVE ( 'NONE', #2035, #3038, #7565, .T. ) ;
#653 = APPLICATION_PROTOCOL_DEFINITION ( 'draft international standard', 'automotive_design', 1998, #5064 ) ;
#654 = CARTESIAN_POINT ( 'NONE',  ( -1.265664690411614835E-16, 2.066987299999999639, 1.850000001092474644 ) ) ;
#655 = CARTESIAN_POINT ( 'NONE',  ( 2.031800924094035195E-13, 6.250000000000000888, 23.49999999999999289 ) ) ;
#656 = CARTESIAN_POINT ( 'NONE',  ( 1.498625850689462968, 228.1261123260860018, 9.788931089129667029 ) ) ;
#657 = CARTESIAN_POINT ( 'NONE',  ( 2.930922878467392856, 5.520395124723619595, 18.50389213124969956 ) ) ;
#658 = ORIENTED_EDGE ( 'NONE', *, *, #14770, .T. ) ;
#659 = CARTESIAN_POINT ( 'NONE',  ( 2.356441885422377425, -0.8834023615831587684, -2.499692266475796121 ) ) ;
#660 = VERTEX_POINT ( 'NONE', #9125 ) ;
#661 = CARTESIAN_POINT ( 'NONE',  ( 5.000000000000000000, 6.123233995736765296E-16, 0.000000000000000000 ) ) ;
#662 = DIRECTION ( 'NONE',  ( -0.000000000000000000, 1.000000000000000000, -0.000000000000000000 ) ) ;
#663 = CARTESIAN_POINT ( 'NONE',  ( 6.105747081304198076, 1.338335777572145613, 23.69973484982322631 ) ) ;
#664 = CARTESIAN_POINT ( 'NONE',  ( 7.490007020835686369, -2.433650805992243260, 5.000000000000004441 ) ) ;
#665 = AXIS2_PLACEMENT_3D ( 'NONE', #12325, #8839, #2782 ) ;
#666 = B_SPLINE_CURVE_WITH_KNOTS ( 'NONE', 3,
 ( #4284, #3090, #14057, #693, #7943, #3165, #8023, #4442, #1965, #6841, #9296, #8106, #12945, #2045, #9700, #7070, #6037, #13342, #14371, #11905, #7151, #2363 ),
 .UNSPECIFIED., .F., .F.,
 ( 4, 2, 2, 2, 2, 2, 2, 2, 2, 2, 4 ),
 ( 0.5000000000000000000, 0.5625000000000006661, 0.5937500000000005551, 0.6250000000000004441, 0.6875000000000004441, 0.7500000000000003331, 0.7812500000000003331, 0.8125000000000002220, 0.8750000000000002220, 0.9375000000000001110, 1.000000000000000000 ),
 .UNSPECIFIED. ) ;
#667 = FACE_BOUND ( 'NONE', #2310, .T. ) ;
#668 = CARTESIAN_POINT ( 'NONE',  ( 4.435347140100977192, -4.403429997944567020, 17.86762589283694069 ) ) ;
#669 = CARTESIAN_POINT ( 'NONE',  ( 1.035533905932739085, -2.500000000000000000, -0.4499999999999998446 ) ) ;
#670 = DIRECTION ( 'NONE',  ( 0.000000000000000000, 0.000000000000000000, 1.000000000000000000 ) ) ;
#671 = CARTESIAN_POINT ( 'NONE',  ( 5.409423237178978106, 2.597448116731099876, 5.615617326986045654 ) ) ;
#672 = PRODUCT_DEFINITION_SHAPE ( 'NONE', 'NONE',  #15737 ) ;
#673 = CARTESIAN_POINT ( 'NONE',  ( -7.420008617947670970E-16, 188.5999999999999943, 9.500000000000001776 ) ) ;
#674 = CARTESIAN_POINT ( 'NONE',  ( -1.813734975128623139, 228.5291423394705532, 7.767584113458720019 ) ) ;
#675 = UNCERTAINTY_MEASURE_WITH_UNIT (LENGTH_MEASURE( 1.000000000000000082E-05 ), #4499, 'distance_accuracy_value', 'NONE');
#676 = FACE_BOUND ( 'NONE', #9747, .T. ) ;
#677 = EDGE_CURVE ( 'NONE', #4035, #7387, #11489, .T. ) ;
#678 = CARTESIAN_POINT ( 'NONE',  ( 1.000082492230908615, 6.169467968613676412, 24.63152538105401845 ) ) ;
#679 = CARTESIAN_POINT ( 'NONE',  ( -2.066987299999999195, -0.8561741729129467293, -1.099999998907525312 ) ) ;
#680 = PRODUCT_RELATED_PRODUCT_CATEGORY ( 'part', '', ( #13002 ) ) ;
#681 = CARTESIAN_POINT ( 'NONE',  ( 2.500000000000000444, 187.1499999999999773, 8.035533905932739529 ) ) ;
#682 = CARTESIAN_POINT ( 'NONE',  ( -2.997451966578608129, 5.485105005465900518, 25.11517780375843500 ) ) ;
#683 = ADVANCED_FACE ( 'NONE', ( #7913 ), #4483, .T. ) ;
#685 = ORIENTED_EDGE ( 'NONE', *, *, #2400, .T. ) ;
#684 = CARTESIAN_POINT ( 'NONE',  ( 2.500000000000000444, 184.7999999999999829, 7.000000000000000000 ) ) ;
#686 = LINE ( 'NONE', #12938, #533 ) ;
#687 = PRODUCT_DEFINITION_FORMATION_WITH_SPECIFIED_SOURCE ( 'ANY', '', #7157, .NOT_KNOWN. ) ;
#688 = AXIS2_PLACEMENT_3D ( 'NONE', #3084, #7934, #12777 ) ;
#689 = CARTESIAN_POINT ( 'NONE',  ( -5.329907877631303137, 2.755840666746359968, 24.23805675996852926 ) ) ;
#690 = CARTESIAN_POINT ( 'NONE',  ( -0.9617334577332378176, 228.2042837055383302, 10.01878807149740602 ) ) ;
#691 = CARTESIAN_POINT ( 'NONE',  ( 0.4407554187462536799, 188.9999999991368895, 4.532388850900320065 ) ) ;
#692 = DIRECTION ( 'NONE',  ( -0.3090169943749579429, 0.9510565162951502005, 0.000000000000000000 ) ) ;
#693 = CARTESIAN_POINT ( 'NONE',  ( -0.8829701019949064422, 227.6750070165890349, 5.300792584290398679 ) ) ;
#694 = CARTESIAN_POINT ( 'NONE',  ( 1.851056454904606685, 228.5003429013454763, 7.684409693542115782 ) ) ;
#695 = CARTESIAN_POINT ( 'NONE',  ( 5.570760634536804368, -2.834026536768245563, 5.262252817217141221 ) ) ;
#696 = CARTESIAN_POINT ( 'NONE',  ( 0.01012247443264182103, 0.4000000000000027978, 2.496776319709509639 ) ) ;
#697 = CARTESIAN_POINT ( 'NONE',  ( -3.011139120916464851, -5.190534000030369910, 30.20068193741825979 ) ) ;
#698 = ORIENTED_EDGE ( 'NONE', *, *, #8097, .F. ) ;
#699 = CARTESIAN_POINT ( 'NONE',  ( -1.461580736456473018, 188.7499999989075263, 5.538419263543527649 ) ) ;
#700 = CONICAL_SURFACE ( 'NONE', #15707, 4.000000000000001776, 0.1745329251994333364 ) ;
#701 = CARTESIAN_POINT ( 'NONE',  ( 1.035533905932738419, 184.6500000000000057, 9.500000000000000000 ) ) ;
#702 = CIRCLE ( 'NONE', #11125, 12.49999999999999822 ) ;
#703 = VERTEX_POINT ( 'NONE', #13060 ) ;
#704 = CARTESIAN_POINT ( 'NONE',  ( -7.490007020835705909, -2.433650805992367161, 5.000000000000004441 ) ) ;
#705 = CARTESIAN_POINT ( 'NONE',  ( -3.632151824460997158, -4.777505256984662552, 3.999950679266885523 ) ) ;
#706 = B_SPLINE_CURVE_WITH_KNOTS ( 'NONE', 3,
 ( #2538, #5748, #880, #8291, #4628, #9861, #6207, #3345, #66, #4931, #3421, #10590, #13505, #15529, #14713, #1407, #2228, #9481 ),
 .UNSPECIFIED., .F., .F.,
 ( 4, 2, 2, 2, 2, 2, 2, 2, 4 ),
 ( 0.003131486019301977716, 0.003522824630466684856, 0.003914163241631391996, 0.004305501852796100003, 0.004696840463960807142, 0.005088179075125514282, 0.005479517686290222289, 0.005870856297454931164, 0.006262194908619639171 ),
 .UNSPECIFIED. ) ;
#707 = CARTESIAN_POINT ( 'NONE',  ( -0.8561741729129458411, -2.066987299999999195, -2.599999998907525534 ) ) ;
#708 = CARTESIAN_POINT ( 'NONE',  ( -3.011139120916544787, 5.190534000030322836, 31.79931806258174376 ) ) ;
#709 = CARTESIAN_POINT ( 'NONE',  ( 3.566234721237973027, 5.134387337253873973, 17.00008258189708954 ) ) ;
#710 = CARTESIAN_POINT ( 'NONE',  ( -1.767766952966369098, 185.0999999999999943, 5.232233047033630235 ) ) ;
#711 = AXIS2_PLACEMENT_3D ( 'NONE', #4234, #3121, #10361 ) ;
#712 = CARTESIAN_POINT ( 'NONE',  ( 5.621197618055776779, -2.101623592078248670, 23.52601979877760030 ) ) ;
#713 = CARTESIAN_POINT ( 'NONE',  ( 4.592425496802573972E-16, -2.500000000000000000, -0.5000000000000000000 ) ) ;
#714 = AXIS2_PLACEMENT_3D ( 'NONE', #9047, #10461, #4336 ) ;
#715 = CARTESIAN_POINT ( 'NONE',  ( 2.500000000000000000, 3.061616997868383141E-16, -1.799999997815050490 ) ) ;
#716 = CARTESIAN_POINT ( 'NONE',  ( -5.999999999999999112, 229.2449477060184222, 9.834870838912449287 ) ) ;
#717 = CYLINDRICAL_SURFACE ( 'NONE', #10044, 0.9999999999999998890 ) ;
#718 = CARTESIAN_POINT ( 'NONE',  ( -5.842988226680535746, -1.369004370660826808, 17.12619317285288645 ) ) ;
#719 = DIRECTION ( 'NONE',  ( -0.5877852522924685852, -0.8090169943749507819, 0.000000000000000000 ) ) ;
#720 = ADVANCED_FACE ( 'NONE', ( #5682 ), #7733, .T. ) ;
#721 = VERTEX_POINT ( 'NONE', #10435 ) ;
#722 = ORIENTED_EDGE ( 'NONE', *, *, #3306, .T. ) ;
#723 = ORIENTED_EDGE ( 'NONE', *, *, #10280, .F. ) ;
#724 =( GEOMETRIC_REPRESENTATION_CONTEXT ( 3 ) GLOBAL_UNCERTAINTY_ASSIGNED_CONTEXT ( ( #15717 ) ) GLOBAL_UNIT_ASSIGNED_CONTEXT ( ( #11873, #5266, #3102 ) ) REPRESENTATION_CONTEXT ( 'NONE', 'WORKASPACE' ) );
#725 = CARTESIAN_POINT ( 'NONE',  ( 2.930600586412987152, -5.520563544161741554, 12.00308643866044100 ) ) ;
#726 = PLANE ( 'NONE',  #3772 ) ;
#727 = VERTEX_POINT ( 'NONE', #4463 ) ;
#728 = CARTESIAN_POINT ( 'NONE',  ( 2.500000000000000444, 184.7999999999999829, 7.000000000000000000 ) ) ;
#729 = ADVANCED_FACE ( 'NONE', ( #11618 ), #5821, .F. ) ;
#730 = CARTESIAN_POINT ( 'NONE',  ( -2.500000000000000444, 1.035533905932737753, 0.1500000021849496601 ) ) ;
#731 = CARTESIAN_POINT ( 'NONE',  ( -0.9735856429310829618, 5.920699391845060333, 24.76285283906726065 ) ) ;
#732 = CARTESIAN_POINT ( 'NONE',  ( -13.50000000000000000, 0.000000000000000000, 2.479909768273400161E-15 ) ) ;
#733 = CARTESIAN_POINT ( 'NONE',  ( -1.035533905932737975, 188.9499999978150697, 4.500000000000000888 ) ) ;
#734 = EDGE_CURVE ( 'NONE', #2516, #15573, #442, .T. ) ;
#735 = CARTESIAN_POINT ( 'NONE',  ( -2.500000000000000000, 0.000000000000000000, 1.706999999978150662 ) ) ;
#736 = LINE ( 'NONE', #2156, #8210 ) ;
#737 = SHAPE_DEFINITION_REPRESENTATION ( #15269, #5305 ) ;
#738 = COLOUR_RGB ( '', 0.66274510, 0.83137255, 0.94901961) ;
#739 = CARTESIAN_POINT ( 'NONE',  ( -1.265664690411614835E-16, 2.066987299999999639, 0.2500000010924746663 ) ) ;
#740 = CARTESIAN_POINT ( 'NONE',  ( -5.782947755040659388, -1.603807858344015402, 4.026019798777604741 ) ) ;
#741 = CARTESIAN_POINT ( 'NONE',  ( 0.09789622041826544219, 228.2551367208810689, 10.16828408546989237 ) ) ;
#742 = CIRCLE ( 'NONE', #2268, 1.499999999999999556 ) ;
#743 = CARTESIAN_POINT ( 'NONE',  ( -1.530808498934191571E-16, 2.500000000000000000, 0.8000000021849498211 ) ) ;
#744 = ORIENTED_EDGE ( 'NONE', *, *, #70, .F. ) ;
#745 = CARTESIAN_POINT ( 'NONE',  ( -2.135032056815611146, -1.308652412870009663, -2.499304978889202555 ) ) ;
#746 = ORIENTED_EDGE ( 'NONE', *, *, #9967, .F. ) ;
#747 = CARTESIAN_POINT ( 'NONE',  ( -0.9740856415300116478, 6.173834621338605722, 11.23852653055529238 ) ) ;
#748 = EDGE_CURVE ( 'NONE', #5121, #5942, #5782, .T. ) ;
#749 = CARTESIAN_POINT ( 'NONE',  ( 1.035533905932738197, 189.3499999978150754, 9.500000000000000000 ) ) ;
#750 = FACE_OUTER_BOUND ( 'NONE', #5902, .T. ) ;
#751 = EDGE_LOOP ( 'NONE', ( #12486, #12526 ) ) ;
#752 = CARTESIAN_POINT ( 'NONE',  ( 4.435347140100961205, 4.403429997944583008, 11.49999999999998224 ) ) ;
#753 = CARTESIAN_POINT ( 'NONE',  ( 0.3272492347489360798, 2.500000000000000000, -2.500000000000000000 ) ) ;
#754 = CARTESIAN_POINT ( 'NONE',  ( 3.568242062701502793, -5.132954954975523343, 16.99995093123465395 ) ) ;
#755 = CARTESIAN_POINT ( 'NONE',  ( 2.500000000000000444, 1.035533905932737975, -1.850000000000000533 ) ) ;
#756 = DIRECTION ( 'NONE',  ( 0.000000000000000000, 1.000000000000000000, 0.000000000000000000 ) ) ;
#757 = FILL_AREA_STYLE_COLOUR ( '', #14472 ) ;
#758 = CARTESIAN_POINT ( 'NONE',  ( -7.490007020835705909, -2.433650805992367161, 5.000000000000004441 ) ) ;
#759 = CARTESIAN_POINT ( 'NONE',  ( -1.035533905932737975, 188.2500000000000000, 4.500000000000000888 ) ) ;
#761 = CARTESIAN_POINT ( 'NONE',  ( -1.987493679921816137, 228.2178828950600860, 6.868649084925799286 ) ) ;
#760 = AXIS2_PLACEMENT_3D ( 'NONE', #2422, #4904, #3847 ) ;
#762 = CARTESIAN_POINT ( 'NONE',  ( 6.176542424588138402, -0.9554180641284093500, 17.86939309276499799 ) ) ;
#763 = AXIS2_PLACEMENT_3D ( 'NONE', #4855, #7470, #14549 ) ;
#764 = CARTESIAN_POINT ( 'NONE',  ( -5.531209434046310491, 2.328189801702683415, 18.87303779027050510 ) ) ;
#765 = CARTESIAN_POINT ( 'NONE',  ( 1.461580736456473018, -1.461580736456472573, -0.04999999890752549608 ) ) ;
#766 = CARTESIAN_POINT ( 'NONE',  ( 1.767766952966369098, 187.2999999999999829, 5.232233047033630235 ) ) ;
#767 = CARTESIAN_POINT ( 'NONE',  ( 2.000000000000001776, 1.500000000000008216, -8.673617379884158732E-16 ) ) ;
#769 = ORIENTED_EDGE ( 'NONE', *, *, #11126, .T. ) ;
#768 = CARTESIAN_POINT ( 'NONE',  ( 7.799024015210637373, -1.482594289697068746, 31.00000000000000000 ) ) ;
#770 = DIRECTION ( 'NONE',  ( 0.8090169943749421222, 0.5877852522924802425, 0.000000000000000000 ) ) ;
#771 = EDGE_CURVE ( 'NONE', #5999, #10225, #9169, .T. ) ;
#772 = AXIS2_PLACEMENT_3D ( 'NONE', #14279, #9143, #11588 ) ;
#773 = DIRECTION ( 'NONE',  ( -1.000000000000000000, 0.000000000000000000, 0.000000000000000000 ) ) ;
#774 = CARTESIAN_POINT ( 'NONE',  ( -0.1991118202061275544, 190.0875178197513549, 4.201689379953633008 ) ) ;
#775 =( LENGTH_UNIT ( ) NAMED_UNIT ( * ) SI_UNIT ( .MILLI., .METRE. ) );
#776 = CARTESIAN_POINT ( 'NONE',  ( 4.592425496802573972E-16, -2.500000000000000000, -0.3999999978150502455 ) ) ;
#777 = CARTESIAN_POINT ( 'NONE',  ( 1.035533905932737975, 184.0800000002185186, 4.500000000000000888 ) ) ;
#778 = CARTESIAN_POINT ( 'NONE',  ( -5.408775798201170382, -2.598833957129641714, 5.613977389430841569 ) ) ;
#779 = CARTESIAN_POINT ( 'NONE',  ( 1.725625307041983136, 227.9349420198840903, 6.051499699527947307 ) ) ;
#780 = FACE_BOUND ( 'NONE', #8537, .T. ) ;
#781 = CARTESIAN_POINT ( 'NONE',  ( 0.05741246108494903189, 0.4000000000000045186, 2.543273608808054753 ) ) ;
#782 = CARTESIAN_POINT ( 'NONE',  ( -1.035533905932738197, -2.500000000000000000, 1.150000002184949466 ) ) ;
#783 = ORIENTED_EDGE ( 'NONE', *, *, #12609, .T. ) ;
#784 = CARTESIAN_POINT ( 'NONE',  ( 5.082197683525802034E-17, 185.2499999989074979, 4.933012699999999029 ) ) ;
#785 = CARTESIAN_POINT ( 'NONE',  ( 3.633127580202252460, 4.776802569231076490, 29.99992038825524432 ) ) ;
#786 = VERTEX_POINT ( 'NONE', #4622 ) ;
#787 = DIRECTION ( 'NONE',  ( 0.8090169943749510040, -0.5877852522924683631, 0.000000000000000000 ) ) ;
#788 = EDGE_CURVE ( 'NONE', #5458, #12720, #7023, .T. ) ;
#789 = CARTESIAN_POINT ( 'NONE',  ( -3.632151824461082423, 4.777505256984600379, 32.00004932073311892 ) ) ;
#790 = CARTESIAN_POINT ( 'NONE',  ( 5.486982057989201245, 2.429327048029852332, 17.20068193741825269 ) ) ;
#791 = CARTESIAN_POINT ( 'NONE',  ( -1.461580736456473018, 185.3499999989074922, 5.538419263543526760 ) ) ;
#792 = EDGE_CURVE ( 'NONE', #15586, #8520, #15272, .T. ) ;
#793 = CARTESIAN_POINT ( 'NONE',  ( -0.2619041840692670209, 6.245686665308512353, 23.52605849433794560 ) ) ;
#794 = CARTESIAN_POINT ( 'NONE',  ( -2.500000000000000000, -1.035533905932739307, -0.5499999978150503788 ) ) ;
#795 = DIRECTION ( 'NONE',  ( 0.000000000000000000, 1.000000000000000000, 0.000000000000000000 ) ) ;
#796 = CARTESIAN_POINT ( 'NONE',  ( 3.659182332138577465E-16, 187.9952603975225713, 3.440894205938198613 ) ) ;
#797 = CARTESIAN_POINT ( 'NONE',  ( 0.2619041840695141010, -6.245686665308502583, 30.02605849433794916 ) ) ;
#798 = DIRECTION ( 'NONE',  ( -0.000000000000000000, 1.000000000000000000, -0.000000000000000000 ) ) ;
#799 = DIRECTION ( 'NONE',  ( 0.000000000000000000, 0.000000000000000000, 1.000000000000000000 ) ) ;
#800 = ORIENTED_EDGE ( 'NONE', *, *, #1934, .T. ) ;
#801 = ORIENTED_EDGE ( 'NONE', *, *, #1804, .T. ) ;
#802 = ORIENTED_EDGE ( 'NONE', *, *, #3118, .F. ) ;
#803 = AXIS2_PLACEMENT_3D ( 'NONE', #2594, #12294, #1393 ) ;
#804 = CARTESIAN_POINT ( 'NONE',  ( -6.176542424588095770, -0.9554180641287002285, 11.36765874365828921 ) ) ;
#805 = PLANE ( 'NONE',  #9364 ) ;
#806 = EDGE_LOOP ( 'NONE', ( #9642, #15273, #10053, #13382 ) ) ;
#807 =( NAMED_UNIT ( * ) PLANE_ANGLE_UNIT ( ) SI_UNIT ( $, .RADIAN. ) );
#808 = CARTESIAN_POINT ( 'NONE',  ( 2.500000000000000000, 3.061616997868383141E-16, 0.6000000021849495324 ) ) ;
#809 = CARTESIAN_POINT ( 'NONE',  ( -5.487348639458855537, -2.428538342494488855, 31.80022217383877248 ) ) ;
#810 = CARTESIAN_POINT ( 'NONE',  ( -4.435347140101010055, -4.403429997944535046, 5.000000000000004441 ) ) ;
#811 = CARTESIAN_POINT ( 'NONE',  ( -1.767766952966369765, 189.1999999978150697, 8.767766952966368876 ) ) ;
#812 = CARTESIAN_POINT ( 'NONE',  ( -1.530808498934191571E-16, 2.500000000000000000, -1.693000000021849916 ) ) ;
#813 = CARTESIAN_POINT ( 'NONE',  ( 2.500000000000000444, 185.4999999978150527, 7.000000000000000000 ) ) ;
#814 = APPLICATION_PROTOCOL_DEFINITION ( 'draft international standard', 'automotive_design', 1998, #5877 ) ;
#815 = CARTESIAN_POINT ( 'NONE',  ( -1.265664690411614835E-16, 2.066987299999999639, 1.050000001092474822 ) ) ;
#816 = AXIS2_PLACEMENT_3D ( 'NONE', #2518, #3778, #4670 ) ;
#817 = B_SPLINE_CURVE_WITH_KNOTS ( 'NONE', 3,
 ( #7421, #9969, #10047, #14663, #2722, #6475, #14577, #8627, #12343, #14895, #3981, #8702, #1438, #6238, #13692, #2486, #3830, #4963 ),
 .UNSPECIFIED., .F., .F.,
 ( 4, 2, 2, 2, 2, 2, 2, 2, 4 ),
 ( 0.003131918686235975191, 0.003523310662250265894, 0.003914702638264556597, 0.004306094614278848168, 0.004697486590293138004, 0.005088878566307429574, 0.005480270542321719410, 0.005871662518336009245, 0.006263054494350298214 ),
 .UNSPECIFIED. ) ;
#818 = CARTESIAN_POINT ( 'NONE',  ( -5.842988226680565944, -1.369004370660702463, 4.126193172852896218 ) ) ;
#819 = CARTESIAN_POINT ( 'NONE',  ( 3.000032282732917555, 227.2742683068891552, 7.282695486718367306 ) ) ;
#820 = CARTESIAN_POINT ( 'NONE',  ( 4.153663429050664213, 4.670992970568477176, 18.79933148907576168 ) ) ;
#821 = ORIENTED_EDGE ( 'NONE', *, *, #13085, .F. ) ;
#822 = CARTESIAN_POINT ( 'NONE',  ( -2.397391504966196241, 0.7648662538461182825, -2.499399845735361225 ) ) ;
#823 =( BOUNDED_CURVE ( )  B_SPLINE_CURVE ( 2, ( #1831, #12882, #13771, #14977, #5431, #11461, #11535, #11617, #4068 ),
 .UNSPECIFIED., .F., .F. ) 
 B_SPLINE_CURVE_WITH_KNOTS ( ( 3, 2, 2, 2, 3 ),
 ( 0.5000000000000000000, 0.5178571428571429047, 0.5357142857142856984, 0.5535714285714286031, 0.5714285714285713969 ),
 .UNSPECIFIED. ) 
 CURVE ( )  GEOMETRIC_REPRESENTATION_ITEM ( )  RATIONAL_B_SPLINE_CURVE ( ( 1.000000000000000000, 0.9238795325112867385, 1.000000000000000000, 0.9238795325112867385, 1.000000000000000000, 0.9238795325112867385, 1.000000000000000000, 0.9238795325112867385, 1.000000000000000000 ) ) 
 REPRESENTATION_ITEM ( '' )  );
#824 = ORIENTED_EDGE ( 'NONE', *, *, #635, .T. ) ;
#825 = CARTESIAN_POINT ( 'NONE',  ( -2.997753866155921543, 5.484939622623787869, 17.38439807107078749 ) ) ;
#826 = CARTESIAN_POINT ( 'NONE',  ( 7.347880347650999152E-16, -6.000000000000000888, 4.000000000000004441 ) ) ;
#827 = DIRECTION ( 'NONE',  ( 0.000000000000000000, -0.000000000000000000, 1.000000000000000000 ) ) ;
#829 = ORIENTED_EDGE ( 'NONE', *, *, #10697, .T. ) ;
#828 = VECTOR ( 'NONE', #12028, 1000.000000000000114 ) ;
#830 = CARTESIAN_POINT ( 'NONE',  ( 4.069800786343749976, 4.744882212776869501, 10.62618035954928075 ) ) ;
#831 = CARTESIAN_POINT ( 'NONE',  ( 0.000000000000000000, 19.99999999999999645, 12.50000000000000355 ) ) ;
#832 = PRESENTATION_STYLE_ASSIGNMENT (( #6370 ) ) ;
#833 = CARTESIAN_POINT ( 'NONE',  ( 2.500000000000000444, 1.035533905932737975, 0.5499999999999999334 ) ) ;
#834 = CYLINDRICAL_SURFACE ( 'NONE', #6184, 1.000000000000000888 ) ;
#835 = CARTESIAN_POINT ( 'NONE',  ( -1.257347874116830337E-14, 0.4000000000000047962, -2.458352573764722937 ) ) ;
#836 =( BOUNDED_CURVE ( )  B_SPLINE_CURVE ( 2, ( #3676, #14327, #3434, #8554, #13378 ),
 .UNSPECIFIED., .F., .F. ) 
 B_SPLINE_CURVE_WITH_KNOTS ( ( 3, 2, 3 ),
 ( 0.8571428571428570953, 0.8750000000000000000, 0.8928571428571429047 ),
 .UNSPECIFIED. ) 
 CURVE ( )  GEOMETRIC_REPRESENTATION_ITEM ( )  RATIONAL_B_SPLINE_CURVE ( ( 1.000000000000000000, 0.9238795325112867385, 1.000000000000000000, 0.9238795325112867385, 1.000000000000000000 ) ) 
 REPRESENTATION_ITEM ( '' )  );
#837 = CARTESIAN_POINT ( 'NONE',  ( 1.035533905932737975, 184.8499999978150754, 4.500000000000000888 ) ) ;
#838 = ADVANCED_FACE ( 'NONE', ( #7404 ), #80, .F. ) ;
#839 = CARTESIAN_POINT ( 'NONE',  ( -0.6401557763822781633, 228.8776351522889172, 8.774051233606112277 ) ) ;
#840 = CARTESIAN_POINT ( 'NONE',  ( 6.172614129015258300, -0.9817721000787353880, 17.73763026556123634 ) ) ;
#841 = CARTESIAN_POINT ( 'NONE',  ( -6.176542424588120639, 0.9554180641285460185, 5.000000000000004441 ) ) ;
#842 = EDGE_CURVE ( 'NONE', #7816, #5381, #5978, .T. ) ;
#843 = CARTESIAN_POINT ( 'NONE',  ( 0.03582210218219494119, 189.0000000000000284, 4.500171129856880725 ) ) ;
#844 = CARTESIAN_POINT ( 'NONE',  ( 2.500000000000000444, 188.0500000000000114, 5.964466094067262247 ) ) ;
#845 = CARTESIAN_POINT ( 'NONE',  ( -1.767766952966369320, 187.3999999978150584, 5.232233047033630235 ) ) ;
#847 = ORIENTED_EDGE ( 'NONE', *, *, #12750, .T. ) ;
#846 = CYLINDRICAL_SURFACE ( 'NONE', #9301, 1.000000000000000888 ) ;
#848 = CARTESIAN_POINT ( 'NONE',  ( 0.000000000000000000, 0.000000000000000000, 2.500000000000000000 ) ) ;
#849 = AXIS2_PLACEMENT_3D ( 'NONE', #732, #12900, #2001 ) ;
#850 = FACE_OUTER_BOUND ( 'NONE', #8632, .T. ) ;
#851 = CARTESIAN_POINT ( 'NONE',  ( -2.781333881087624249, 226.9279571253883319, 6.262926915399051886 ) ) ;
#852 =( NAMED_UNIT ( * ) SI_UNIT ( $, .STERADIAN. ) SOLID_ANGLE_UNIT ( ) );
#853 = CARTESIAN_POINT ( 'NONE',  ( -5.131373506000715068, 7.062729720844030723, 5.000000000000004441 ) ) ;
#854 = CARTESIAN_POINT ( 'NONE',  ( 7.490007020835706797, -2.433650805992179755, 11.49999999999998224 ) ) ;
#855 = CARTESIAN_POINT ( 'NONE',  ( -0.5044069930203080032, 5.979990686694993229, 31.87335743227904317 ) ) ;
#856 = CARTESIAN_POINT ( 'NONE',  ( 1.362382138968808887, 227.7849605967929847, 5.618344795260735935 ) ) ;
#857 = FACE_BOUND ( 'NONE', #1667, .T. ) ;
#858 = CARTESIAN_POINT ( 'NONE',  ( -6.155867707731125016, 1.081837891425820430, 4.495630303198471900 ) ) ;
#859 = LINE ( 'NONE', #9458, #13806 ) ;
#860 = VERTEX_POINT ( 'NONE', #7173 ) ;
#861 = CARTESIAN_POINT ( 'NONE',  ( 2.066987299999999639, 189.2499999989075263, 7.000000000000000000 ) ) ;
#862 = CARTESIAN_POINT ( 'NONE',  ( 4.005785023174439630, 4.467917056767417350, 30.20047945897283981 ) ) ;
#863 = ORIENTED_EDGE ( 'NONE', *, *, #9514, .T. ) ;
#864 = CARTESIAN_POINT ( 'NONE',  ( 2.500000000000000444, 186.4000000000000057, 7.000000000000000000 ) ) ;
#865 = CARTESIAN_POINT ( 'NONE',  ( 1.461580736456473018, 185.3499999989075206, 5.538419263543527649 ) ) ;
#866 = CARTESIAN_POINT ( 'NONE',  ( 0.000000000000000000, 2.000000000000000000, -2.500000000000000000 ) ) ;
#867 = CARTESIAN_POINT ( 'NONE',  ( -9.825582188149883933E-17, 187.6499999989075320, 4.933012699999999029 ) ) ;
#868 = CARTESIAN_POINT ( 'NONE',  ( 5.935543223013889147, -0.8771126767604601193, 24.49999999999999289 ) ) ;
#869 = EDGE_CURVE ( 'NONE', #11793, #278, #11659, .T. ) ;
#870 = CARTESIAN_POINT ( 'NONE',  ( -1.035533905932738197, -2.500000000000000000, 1.150000002184949466 ) ) ;
#871 = CARTESIAN_POINT ( 'NONE',  ( -5.558508435838188433, -2.857531096718932684, 5.000000000000004441 ) ) ;
#872 = CARTESIAN_POINT ( 'NONE',  ( 3.659182332138577465E-16, 195.9172377311516016, 6.220370292208427188 ) ) ;
#873 = CARTESIAN_POINT ( 'NONE',  ( -2.500000000000000000, 0.000000000000000000, 0.9000000000000000222 ) ) ;
#874 = CARTESIAN_POINT ( 'NONE',  ( 2.817313151351089395, 5.579000502529482652, 31.13063932754212004 ) ) ;
#875 = DIRECTION ( 'NONE',  ( -6.123233995736766036E-17, 1.000000000000000000, 0.000000000000000000 ) ) ;
#876 = ORIENTED_EDGE ( 'NONE', *, *, #267, .F. ) ;
#877 = EDGE_CURVE ( 'NONE', #5381, #5666, #1680, .T. ) ;
#878 = VERTEX_POINT ( 'NONE', #12172 ) ;
#879 = ORIENTED_EDGE ( 'NONE', *, *, #5328, .F. ) ;
#880 = CARTESIAN_POINT ( 'NONE',  ( 2.841163418881370362, 5.567120626447941589, 30.73763026556126476 ) ) ;
#881 = CARTESIAN_POINT ( 'NONE',  ( 1.002352689154774934, 228.8297273714526625, 8.635690830070354096 ) ) ;
#882 = ORIENTED_EDGE ( 'NONE', *, *, #3262, .T. ) ;
#883 = CARTESIAN_POINT ( 'NONE',  ( -2.500000000000000000, -1.035533905932739307, -0.5499999978150504898 ) ) ;
#884 = CARTESIAN_POINT ( 'NONE',  ( 0.8736516769106962288, -5.936271176698232566, 4.496067715786787211 ) ) ;
#885 = CARTESIAN_POINT ( 'NONE',  ( -3.158825713737453800, -5.393784879207189853, 4.200668510924231214 ) ) ;
#886 = CARTESIAN_POINT ( 'NONE',  ( 0.8561741729129461742, 185.0999999989074922, 9.066987299999999195 ) ) ;
#887 = CARTESIAN_POINT ( 'NONE',  ( 1.035533905932739085, -2.500000000000000000, -0.4430000000218494716 ) ) ;
#888 = CARTESIAN_POINT ( 'NONE',  ( 6.155973317223288888, -1.081218830693701394, 4.496913561339538568 ) ) ;
#889 = APPLICATION_PROTOCOL_DEFINITION ( 'draft international standard', 'automotive_design', 1998, #15421 ) ;
#890 = CARTESIAN_POINT ( 'NONE',  ( 1.461580736456473018, -1.461580736456472573, 1.550000001092474822 ) ) ;
#891 = CARTESIAN_POINT ( 'NONE',  ( -5.330004929009576564, -2.755647751839420234, 4.737601081944046832 ) ) ;
#892 = CARTESIAN_POINT ( 'NONE',  ( 2.998712701283978710, 227.3219367242041926, 7.423021690895281743 ) ) ;
#893 = CARTESIAN_POINT ( 'NONE',  ( -1.238695443643032412, 228.1695118093442716, 9.916540120957755278 ) ) ;
#894 = EDGE_LOOP ( 'NONE', ( #6085, #14105 ) ) ;
#895 = CIRCLE ( 'NONE', #8543, 2.483389555546411831 ) ;
#896 = CARTESIAN_POINT ( 'NONE',  ( -4.000000000000002665, 184.0000000000000000, -7.000000000000000000 ) ) ;
#897 = MECHANICAL_DESIGN_GEOMETRIC_PRESENTATION_REPRESENTATION (  '', ( #8272 ), #8792 ) ;
#898 = VERTEX_POINT ( 'NONE', #13447 ) ;
#899 = CARTESIAN_POINT ( 'NONE',  ( 0.8499999999999896527, 0.000000000000000000, 0.000000000000000000 ) ) ;
#900 = LINE ( 'NONE', #8075, #8869 ) ;
#901 = FACE_BOUND ( 'NONE', #10404, .T. ) ;
#902 = VERTEX_POINT ( 'NONE', #11057 ) ;
#903 = CARTESIAN_POINT ( 'NONE',  ( 2.817313151351048539, 5.579000502529503969, 11.36939309276499088 ) ) ;
#904 = UNCERTAINTY_MEASURE_WITH_UNIT (LENGTH_MEASURE( 1.000000000000000082E-05 ), #8679, 'distance_accuracy_value', 'NONE');
#905 = CARTESIAN_POINT ( 'NONE',  ( 3.421280866380972618, 4.930711975951031611, 25.50004932073312247 ) ) ;
#906 = FACE_BOUND ( 'NONE', #12968, .T. ) ;
#907 = CARTESIAN_POINT ( 'NONE',  ( 0.000000000000000000, 0.000000000000000000, 0.000000000000000000 ) ) ;
#908 = CARTESIAN_POINT ( 'NONE',  ( -2.500000000000000000, -1.035533905932739307, 0.9499999999999999556 ) ) ;
#909 = DIRECTION ( 'NONE',  ( 0.000000000000000000, -2.775557561562887900E-16, 1.000000000000000000 ) ) ;
#910 = CARTESIAN_POINT ( 'NONE',  ( 0.01536757896558604841, 0.4000000000000027978, -2.504920264071737179 ) ) ;
#911 = CARTESIAN_POINT ( 'NONE',  ( 2.500000000000000444, 185.5499999978150640, 5.964466094067262247 ) ) ;
#912 = CARTESIAN_POINT ( 'NONE',  ( -1.785671180686238868, 228.5485690224869586, 7.823689482036285447 ) ) ;
#913 = CARTESIAN_POINT ( 'NONE',  ( -5.726307184802590378, -2.506131700382607352, 18.80026515017675592 ) ) ;
#914 =( BOUNDED_CURVE ( )  B_SPLINE_CURVE ( 2, ( #2367, #1402, #6046, #2449, #8594, #10887, #8350, #11039, #13269 ),
 .UNSPECIFIED., .F., .F. ) 
 B_SPLINE_CURVE_WITH_KNOTS ( ( 3, 2, 2, 2, 3 ),
 ( 0.1428571428571428492, 0.1607142857142857262, 0.1785714285714285754, 0.1964285714285714246, 0.2142857142857142738 ),
 .UNSPECIFIED. ) 
 CURVE ( )  GEOMETRIC_REPRESENTATION_ITEM ( )  RATIONAL_B_SPLINE_CURVE ( ( 1.000000000000000000, 0.9238795325112867385, 1.000000000000000000, 0.9238795325112867385, 1.000000000000000000, 0.9238795325112867385, 1.000000000000000000, 0.9238795325112867385, 1.000000000000000000 ) ) 
 REPRESENTATION_ITEM ( '' )  );
#915 = CARTESIAN_POINT ( 'NONE',  ( -0.1354819475358782221, 189.4421779970482760, 3.974290229956241038 ) ) ;
#916 = CARTESIAN_POINT ( 'NONE',  ( 1.035533905932737753, 186.5499999999999829, 4.500000000000000888 ) ) ;
#917 = CARTESIAN_POINT ( 'NONE',  ( 4.153440676704338586, -4.671190581744546932, 25.29954462468842635 ) ) ;
#918 = AXIS2_PLACEMENT_3D ( 'NONE', #466, #15034, #6295 ) ;
#920 = VERTEX_POINT ( 'NONE', #156 ) ;
#919 = DIRECTION ( 'NONE',  ( 0.000000000000000000, 1.000000000000000000, 0.000000000000000000 ) ) ;
#921 = CARTESIAN_POINT ( 'NONE',  ( -6.155854678529465218, 1.081900940642161135, 18.50425949503010159 ) ) ;
#922 = ORIENTED_EDGE ( 'NONE', *, *, #11635, .F. ) ;
#923 = EDGE_CURVE ( 'NONE', #15371, #5418, #15489, .T. ) ;
#924 = CARTESIAN_POINT ( 'NONE',  ( -5.408775798201112650, 2.598833957129762950, 23.88602261056918152 ) ) ;
#925 = CARTESIAN_POINT ( 'NONE',  ( -2.774519402982507543, 226.9225964823893378, 6.247138756163614914 ) ) ;
#926 = PRESENTATION_STYLE_ASSIGNMENT (( #5953 ) ) ;
#927 = CARTESIAN_POINT ( 'NONE',  ( 1.616071383507818870, 190.0421234246860820, 4.677467377199475251 ) ) ;
#928 = CARTESIAN_POINT ( 'NONE',  ( -2.500000000000000444, 184.3800000002184731, 8.035533905932737753 ) ) ;
#929 = CARTESIAN_POINT ( 'NONE',  ( -9.750000000000003553, 22.00000000000000000, -1.500000000000033751 ) ) ;
#930 = AXIS2_PLACEMENT_3D ( 'NONE', #4602, #8185, #8263 ) ;
#931 = CARTESIAN_POINT ( 'NONE',  ( 1.050562149602352946, 228.8138732705275231, 8.589903282340008772 ) ) ;
#932 = FACE_BOUND ( 'NONE', #5455, .T. ) ;
#933 = CARTESIAN_POINT ( 'NONE',  ( 1.461580736456473018, -1.461580736456472573, 1.750000001092474999 ) ) ;
#934 = DIRECTION ( 'NONE',  ( -6.123233995736766036E-17, 1.000000000000000000, 0.000000000000000000 ) ) ;
#935 = ORIENTED_EDGE ( 'NONE', *, *, #8740, .F. ) ;
#936 = CARTESIAN_POINT ( 'NONE',  ( -2.066987300000001415, 188.8999999989075320, 7.856174172912944620 ) ) ;
#937 = PRODUCT_DEFINITION_SHAPE ( 'NONE', 'NONE',  #15766 ) ;
#938 = CARTESIAN_POINT ( 'NONE',  ( 3.922396193919027496, 4.541970110199465616, 30.12619317285289711 ) ) ;
#939 = EDGE_CURVE ( 'NONE', #12601, #2089, #13670, .T. ) ;
#940 = B_SPLINE_CURVE_WITH_KNOTS ( 'NONE', 3,
 ( #9001, #2705, #7790, #12637, #4049, #1737, #6532, #468, #12403, #8920, #7555, #11520, #1503, #11213, #2862, #10182, #4129, #4211 ),
 .UNSPECIFIED., .F., .F.,
 ( 4, 2, 2, 2, 2, 2, 2, 2, 4 ),
 ( 0.003131918686235973890, 0.003523310662250264159, 0.003914702638264553995, 0.004306094614278844698, 0.004697486590293134534, 0.005088878566307424370, 0.005480270542321714206, 0.005871662518336004041, 0.006263054494350294744 ),
 .UNSPECIFIED. ) ;
#941 = ORIENTED_EDGE ( 'NONE', *, *, #5328, .T. ) ;
#942 = CARTESIAN_POINT ( 'NONE',  ( -3.311384659207067038, -5.004923837169465983, 4.026414045633067040 ) ) ;
#943 = EDGE_CURVE ( 'NONE', #2947, #7387, #83, .T. ) ;
#944 = CARTESIAN_POINT ( 'NONE',  ( -4.286401442266607020, 4.198423832313117110, 31.00000000000000000 ) ) ;
#945 = CARTESIAN_POINT ( 'NONE',  ( 5.915699123067176934, 1.003533581835446276, 17.49610204984016804 ) ) ;
#946 = CARTESIAN_POINT ( 'NONE',  ( -0.8561741729129457301, 185.2999999989075661, 4.933012699999999029 ) ) ;
#947 = B_SPLINE_CURVE_WITH_KNOTS ( 'NONE', 3,
 ( #4040, #8914, #2855, #6525, #11512, #2696, #306, #1805, #5332, #6371, #9943, #10176, #7547, #15028, #12394, #6679, #11205, #5167 ),
 .UNSPECIFIED., .F., .F.,
 ( 4, 2, 2, 2, 2, 2, 2, 2, 4 ),
 ( 0.000000000000000000, 0.0003914898357794960857, 0.0007829796715589921715, 0.001174469507338488095, 0.001565959343117984343, 0.001957449178897481025, 0.002348939014676977924, 0.002740428850456474389, 0.003131918686235971288 ),
 .UNSPECIFIED. ) ;
#948 = FACE_OUTER_BOUND ( 'NONE', #587, .T. ) ;
#949 = CARTESIAN_POINT ( 'NONE',  ( -2.500000000000000444, 1.035533905932737753, -0.6499999978150502455 ) ) ;
#950 = CARTESIAN_POINT ( 'NONE',  ( 4.286401442266545736, -4.198423832313181059, 11.36760611998364467 ) ) ;
#951 = CARTESIAN_POINT ( 'NONE',  ( -5.999999999999999112, 187.2933328889893403, 9.583808270834989429 ) ) ;
#952 = CARTESIAN_POINT ( 'NONE',  ( -1.097593809647108287, 189.0000000000000000, 9.257041379597499287 ) ) ;
#953 = CARTESIAN_POINT ( 'NONE',  ( -1.767766952966369098, 1.767766952966369098, 0.7999999999999999334 ) ) ;
#954 = CARTESIAN_POINT ( 'NONE',  ( 2.817313151351089839, 5.579000502529481764, 31.00000000000000000 ) ) ;
#955 = DIRECTION ( 'NONE',  ( 1.000000000000000000, 6.123233995736766036E-17, 0.000000000000000000 ) ) ;
#956 = AXIS2_PLACEMENT_3D ( 'NONE', #13283, #2700, #14724 ) ;
#957 = ORIENTED_EDGE ( 'NONE', *, *, #9756, .T. ) ;
#958 = ADVANCED_FACE ( 'NONE', ( #14875 ), #237, .F. ) ;
#959 = ORIENTED_EDGE ( 'NONE', *, *, #1371, .T. ) ;
#960 = ORIENTED_EDGE ( 'NONE', *, *, #11186, .T. ) ;
#961 = CARTESIAN_POINT ( 'NONE',  ( -0.8561741729129467293, 184.9999999989074979, 9.066987299999999195 ) ) ;
#962 = CYLINDRICAL_SURFACE ( 'NONE', #2245, 1.000000000000000888 ) ;
#963 = ORIENTED_EDGE ( 'NONE', *, *, #15525, .T. ) ;
#964 = CARTESIAN_POINT ( 'NONE',  ( 2.066987300000000083, -0.8561741729129449530, 1.600000001092474644 ) ) ;
#965 = CARTESIAN_POINT ( 'NONE',  ( 0.8002302970946603144, -5.947135855825864681, 4.386017732123007384 ) ) ;
#966 = CARTESIAN_POINT ( 'NONE',  ( 9.750000000000003553, 22.00000000000000000, 1.500000000000101696 ) ) ;
#967 = CARTESIAN_POINT ( 'NONE',  ( -0.8561741729129455081, 186.2999999989075093, 4.933012699999999029 ) ) ;
#968 = EDGE_CURVE ( 'NONE', #3363, #12097, #1421, .T. ) ;
#969 = CARTESIAN_POINT ( 'NONE',  ( -1.530808498934191571E-16, 2.500000000000000000, -0.8930000000218497602 ) ) ;
#970 = CARTESIAN_POINT ( 'NONE',  ( -7.180990026460747799, -3.384707322287517695, 5.000000000000004441 ) ) ;
#971 = ITEM_DEFINED_TRANSFORMATION ( 'NONE', 'NONE', #13721,  #14201 ) ;
#972 = CARTESIAN_POINT ( 'NONE',  ( 0.8561741729129463963, -2.066987299999999195, 1.500000001092474555 ) ) ;
#973 = CARTESIAN_POINT ( 'NONE',  ( 3.459597053047906989, -5.206576120509703642, 30.02591457665829466 ) ) ;
#974 = CARTESIAN_POINT ( 'NONE',  ( 2.257611286988003396, 226.6535225833466427, 5.454435118953909978 ) ) ;
#975 = CARTESIAN_POINT ( 'NONE',  ( 5.940390500375535510, 6.474944468551633747, 31.00000000000000000 ) ) ;
#976 = ADVANCED_FACE ( 'NONE', ( #7709 ), #3965, .F. ) ;
#977 = CIRCLE ( 'NONE', #711, 2.000000000000000000 ) ;
#978 = ORIENTED_EDGE ( 'NONE', *, *, #14189, .T. ) ;
#979 = CARTESIAN_POINT ( 'NONE',  ( 2.782468714962460510, -5.316055268221388630, 4.496102049840168036 ) ) ;
#980 = ORIENTED_EDGE ( 'NONE', *, *, #10036, .F. ) ;
#981 = ORIENTED_EDGE ( 'NONE', *, *, #4957, .F. ) ;
#982 = CARTESIAN_POINT ( 'NONE',  ( 0.000000000000000000, 6.250000000000000888, 32.00000000000000000 ) ) ;
#983 = CARTESIAN_POINT ( 'NONE',  ( 3.736691294293403409, -4.695920479336392894, 17.02641404563305372 ) ) ;
#984 = DIRECTION ( 'NONE',  ( -0.000000000000000000, 1.000000000000000000, -0.000000000000000000 ) ) ;
#985 = ORIENTED_EDGE ( 'NONE', *, *, #7956, .T. ) ;
#986 = CARTESIAN_POINT ( 'NONE',  ( 3.633127580202278661, -4.776802569231053397, 12.50007961174474502 ) ) ;
#987 = CYLINDRICAL_SURFACE ( 'NONE', #1712, 2.500000000000000000 ) ;
#988 = AXIS2_PLACEMENT_3D ( 'NONE', #396, #13994, #10114 ) ;
#989 = CARTESIAN_POINT ( 'NONE',  ( -0.7988860301920154283, -6.199427171881362497, 23.88455580536193423 ) ) ;
#990 = CARTESIAN_POINT ( 'NONE',  ( 0.000000000000000000, 184.0000000000000000, 2.999999999999998224 ) ) ;
#991 = CARTESIAN_POINT ( 'NONE',  ( 0.8002302970947927641, -5.947135855825846917, 17.38601773212298696 ) ) ;
#992 = DIRECTION ( 'NONE',  ( 0.9510565162951500895, 0.3090169943749582204, 0.000000000000000000 ) ) ;
#993 = EDGE_CURVE ( 'NONE', #12662, #9246, #11351, .T. ) ;
#994 = CARTESIAN_POINT ( 'NONE',  ( 5.375913338529056062, 2.664979843780506563, 5.504289203620185589 ) ) ;
#995 = CARTESIAN_POINT ( 'NONE',  ( 2.500000000000000000, 188.0000000000000000, 7.000000000000000000 ) ) ;
#996 = CARTESIAN_POINT ( 'NONE',  ( 1.455795469679321608, 228.1339131991090596, 9.811868761735363265 ) ) ;
#997 = CARTESIAN_POINT ( 'NONE',  ( 5.558508435838291462, -2.857531096718732400, 17.99999999999998934 ) ) ;
#998 = CARTESIAN_POINT ( 'NONE',  ( 0.07162669437691278340, 189.0000000000000000, 4.501026287322612340 ) ) ;
#999 = AXIS2_PLACEMENT_3D ( 'NONE', #13899, #6603, #9146 ) ;
#1000 = ORIENTED_EDGE ( 'NONE', *, *, #3749, .T. ) ;
#1001 = CARTESIAN_POINT ( 'NONE',  ( -3.420311045507830272, 4.931422832349302787, 3.999920388255239434 ) ) ;
#1002 = CARTESIAN_POINT ( 'NONE',  ( -0.9737778612004891476, -5.920671847850528025, 11.23736375884651473 ) ) ;
#1004 = VERTEX_POINT ( 'NONE', #11365 ) ;
#1003 = CARTESIAN_POINT ( 'NONE',  ( -1.767766952966369098, 1.767766952966369098, -1.499999997815050001 ) ) ;
#1005 = CYLINDRICAL_SURFACE ( 'NONE', #3266, 20.00000000000000000 ) ;
#1006 = CARTESIAN_POINT ( 'NONE',  ( 0.3133709289735966963, 0.4000000000000062395, 2.571515392583430426 ) ) ;
#1007 = CARTESIAN_POINT ( 'NONE',  ( -5.409007216690667974, -2.598315788643760893, 30.38557478428061032 ) ) ;
#1008 =( REPRESENTATION_RELATIONSHIP ('NONE','NONE', #11191, #3660 ) REPRESENTATION_RELATIONSHIP_WITH_TRANSFORMATION ( #12263 )SHAPE_REPRESENTATION_RELATIONSHIP( ) );
#1009 = CARTESIAN_POINT ( 'NONE',  ( -2.066987299999999639, 0.8561741729129452860, 1.400000001092474911 ) ) ;
#1010 = CARTESIAN_POINT ( 'NONE',  ( -2.999884802989111421, 227.2993432378640932, 7.356512168893465820 ) ) ;
#1011 =( NAMED_UNIT ( * ) PLANE_ANGLE_UNIT ( ) SI_UNIT ( $, .RADIAN. ) );
#1012 = CARTESIAN_POINT ( 'NONE',  ( 5.558508435838282580, 2.857531096718751940, 24.63234125634168237 ) ) ;
#1013 = CARTESIAN_POINT ( 'NONE',  ( -1.767766952966369542, 184.4300000002185129, 8.767766952966368876 ) ) ;
#1014 = LINE ( 'NONE', #2445, #12121 ) ;
#1015 = CARTESIAN_POINT ( 'NONE',  ( -1.986723294250032357, 228.3028615258686500, 7.114072217564876510 ) ) ;
#1016 = FACE_BOUND ( 'NONE', #8827, .T. ) ;
#1017 = CARTESIAN_POINT ( 'NONE',  ( -1.461580736456472795, 1.461580736456472795, -1.049999998907525045 ) ) ;
#1018 = CARTESIAN_POINT ( 'NONE',  ( -2.500000000000000000, 0.000000000000000000, -1.399999997815050357 ) ) ;
#1019 = ORIENTED_EDGE ( 'NONE', *, *, #5618, .F. ) ;
#1020 = CARTESIAN_POINT ( 'NONE',  ( 0.8561741729129460632, 188.0999999989074922, 9.066987300000000971 ) ) ;
#1021 = CARTESIAN_POINT ( 'NONE',  ( 5.665824935993652112, 1.978765057080799306, 23.50004946353776702 ) ) ;
#1022 = VERTEX_POINT ( 'NONE', #10181 ) ;
#1023 = CARTESIAN_POINT ( 'NONE',  ( 2.500000000000000444, 186.3499999999999943, 8.035533905932739529 ) ) ;
#1024 = CARTESIAN_POINT ( 'NONE',  ( 0.8738043859792735679, -6.188821459035850125, 25.00341560223748871 ) ) ;
#1025 = CARTESIAN_POINT ( 'NONE',  ( -3.107688324358719889, 5.133887830459828550, 31.87378430870261425 ) ) ;
#1026 = CARTESIAN_POINT ( 'NONE',  ( -2.500000000000000444, 186.6999999978150697, 7.000000000000000000 ) ) ;
#1027 = CARTESIAN_POINT ( 'NONE',  ( -0.8561741729129469514, 186.3999999989075320, 9.066987300000000971 ) ) ;
#1028 = CARTESIAN_POINT ( 'NONE',  ( 3.736691294293317700, 4.695920479336459508, 18.97358595436693207 ) ) ;
#1029 = CARTESIAN_POINT ( 'NONE',  ( 1.035533905932737531, 2.500000000000000444, -1.649999997815050357 ) ) ;
#1030 = CARTESIAN_POINT ( 'NONE',  ( 3.632753594129332964, -4.777047695050978149, 10.50004946353775281 ) ) ;
#1031 = CARTESIAN_POINT ( 'NONE',  ( 9.750000000000003553, 22.00000000000000000, 1.500000000000101696 ) ) ;
#1032 = CARTESIAN_POINT ( 'NONE',  ( 0.1306394121199586922, -6.250000000000000888, 30.00000000000000355 ) ) ;
#1033 = CARTESIAN_POINT ( 'NONE',  ( 5.375886393124341467, 2.665038680141373906, 4.495602393557859955 ) ) ;
#1034 = CARTESIAN_POINT ( 'NONE',  ( -0.1323602877610810247, -6.000000000000004441, 18.99999999999998224 ) ) ;
#1035 = EDGE_CURVE ( 'NONE', #3171, #11235, #11462, .T. ) ;
#1036 = VERTEX_POINT ( 'NONE', #6610 ) ;
#1037 = ADVANCED_FACE ( 'NONE', ( #2861 ), #6531, .F. ) ;
#1038 = ORIENTED_EDGE ( 'NONE', *, *, #14388, .F. ) ;
#1039 = B_SPLINE_CURVE_WITH_KNOTS ( 'NONE', 3,
 ( #8427, #10958, #13183, #15581, #2282, #6993, #5956, #10800, #15659, #4760, #9617, #56, #11822, #14456, #3636, #3559, #10642, #9375 ),
 .UNSPECIFIED., .F., .F.,
 ( 4, 2, 2, 2, 2, 2, 2, 2, 4 ),
 ( 0.000000000000000000, 0.0003914357524127484072, 0.0007828715048254968143, 0.001174307257238245330, 0.001565743009650993629, 0.001957178762063741927, 0.002348614514476490660, 0.002740050266889238959, 0.003131486019301987257 ),
 .UNSPECIFIED. ) ;
#1040 = VERTEX_POINT ( 'NONE', #4128 ) ;
#1041 = CARTESIAN_POINT ( 'NONE',  ( -2.066987300000000083, 185.5999999989075491, 6.143825827087054492 ) ) ;
#1042 = DIRECTION ( 'NONE',  ( 0.000000000000000000, 1.000000000000000000, 0.000000000000000000 ) ) ;
#1043 = EDGE_CURVE ( 'NONE', #4972, #8636, #4494, .T. ) ;
#1044 = ORIENTED_EDGE ( 'NONE', *, *, #4453, .F. ) ;
#1045 = CARTESIAN_POINT ( 'NONE',  ( -2.500000000000000444, 1.035533905932737753, -1.449999997815050623 ) ) ;
#1046 = CARTESIAN_POINT ( 'NONE',  ( 6.172614129015243201, 0.9817721000788186547, 18.26236973443873168 ) ) ;
#1047 = LINE ( 'NONE', #5910, #8971 ) ;
#1048 = CARTESIAN_POINT ( 'NONE',  ( 2.066987299999999195, 188.3999999989075036, 7.856174172912946396 ) ) ;
#1049 = CARTESIAN_POINT ( 'NONE',  ( 1.035533905932737531, 2.500000000000000444, -0.9430000000218496936 ) ) ;
#1050 = DIRECTION ( 'NONE',  ( -0.5877852522924685852, -0.8090169943749508930, 0.000000000000000000 ) ) ;
#1051 = CONTEXT_DEPENDENT_SHAPE_REPRESENTATION ( #1008, #10858 ) ;
#1052 = CARTESIAN_POINT ( 'NONE',  ( -1.265664690411614835E-16, 2.066987299999999639, -2.149999998907525800 ) ) ;
#1053 = LINE ( 'NONE', #4803, #11886 ) ;
#1054 = CARTESIAN_POINT ( 'NONE',  ( 2.191560967657306680, 226.6301005958437145, 5.385416860794732585 ) ) ;
#1055 = DIRECTION ( 'NONE',  ( -0.5877852522924685852, -0.8090169943749507819, 0.000000000000000000 ) ) ;
#1056 = ORIENTED_EDGE ( 'NONE', *, *, #13482, .T. ) ;
#1057 = VECTOR ( 'NONE', #10344, 1000.000000000000000 ) ;
#1058 = ORIENTED_EDGE ( 'NONE', *, *, #6301, .F. ) ;
#1059 = DIRECTION ( 'NONE',  ( 1.000000000000000000, -3.326610055774637112E-18, -1.062480551894331163E-17 ) ) ;
#1060 = ORIENTED_EDGE ( 'NONE', *, *, #4196, .F. ) ;
#1061 = VERTEX_POINT ( 'NONE', #12635 ) ;
#1062 = CARTESIAN_POINT ( 'NONE',  ( -5.903061651806595478, -2.057626436184814001, 30.00008258189710730 ) ) ;
#1063 = CARTESIAN_POINT ( 'NONE',  ( 3.632753594129279673, -4.777047695051020781, 17.00004946353776702 ) ) ;
#1064 = CARTESIAN_POINT ( 'NONE',  ( -4.006441409774807560, -4.467329318258149939, 25.29888242247940155 ) ) ;
#1065 = CARTESIAN_POINT ( 'NONE',  ( -5.558508435838177775, -2.857531096718951780, 31.13063932754212004 ) ) ;
#1066 = CARTESIAN_POINT ( 'NONE',  ( -0.6144300524833572474, -6.220417338033053412, 4.200333721759340833 ) ) ;
#1067 = EDGE_CURVE ( 'NONE', #2087, #12811, #1735, .T. ) ;
#1068 = CARTESIAN_POINT ( 'NONE',  ( -3.923477796648549010, -4.541042560386451044, 12.37303779027049444 ) ) ;
#1069 = FACE_OUTER_BOUND ( 'NONE', #8290, .T. ) ;
#1070 = CARTESIAN_POINT ( 'NONE',  ( 0.8499999999999896527, -4.137240605787344953E-16, 2.649388036945189207 ) ) ;
#1071 = CARTESIAN_POINT ( 'NONE',  ( -4.070863287254225860, -4.743975846881679281, 25.37305891554299819 ) ) ;
#1072 = CARTESIAN_POINT ( 'NONE',  ( 0.000000000000000000, 102.0000000000000142, 0.000000000000000000 ) ) ;
#1073 = EDGE_CURVE ( 'NONE', #9955, #9045, #3815, .T. ) ;
#1074 = PRODUCT_DEFINITION_SHAPE ( 'NONE', 'NONE',  #15756 ) ;
#1075 = CARTESIAN_POINT ( 'NONE',  ( -1.035533905932739751, 188.4499999978150413, 9.500000000000003553 ) ) ;
#1076 = CARTESIAN_POINT ( 'NONE',  ( 2.441738273555474681, 226.7282248110694809, 5.674544857840881029 ) ) ;
#1077 = CARTESIAN_POINT ( 'NONE',  ( 4.195842658231466515, 4.289229542213170987, 31.50439760644212939 ) ) ;
#1078 = CARTESIAN_POINT ( 'NONE',  ( -2.102556124205833044, 189.0000000003525997, 5.635613679834785117 ) ) ;
#1079 = EDGE_CURVE ( 'NONE', #14331, #15449, #9378, .T. ) ;
#1080 = AXIS2_PLACEMENT_3D ( 'NONE', #13512, #14641, #13442 ) ;
#1081 = EDGE_LOOP ( 'NONE', ( #14981, #4075, #14585, #5983 ) ) ;
#1082 = CARTESIAN_POINT ( 'NONE',  ( -2.849573632035255599, 5.280958870664612448, 4.384382673013949017 ) ) ;
#1083 = CARTESIAN_POINT ( 'NONE',  ( 0.7993282387951774481, -5.947240459526499379, 12.11484358216955393 ) ) ;
#1085 = ORIENTED_EDGE ( 'NONE', *, *, #3214, .F. ) ;
#1084 = CARTESIAN_POINT ( 'NONE',  ( 2.500000000000000000, 3.061616997868383141E-16, -1.100000000000000311 ) ) ;
#1086 = CARTESIAN_POINT ( 'NONE',  ( 0.002340087947992566201, -0.3999999999999958589, 2.475597248086677915 ) ) ;
#1087 = CARTESIAN_POINT ( 'NONE',  ( 2.658620627125748204, 226.8422998350077080, 6.010601022363255552 ) ) ;
#1088 = CARTESIAN_POINT ( 'NONE',  ( -2.668367453516768517, 5.373994336898062940, 11.36763921416086198 ) ) ;
#1089 = CARTESIAN_POINT ( 'NONE',  ( 1.461580736456472573, 1.461580736456472795, 1.150000001092474911 ) ) ;
#1090 = CARTESIAN_POINT ( 'NONE',  ( -2.985771267271970064, 227.3851189813470910, 7.609035584520301043 ) ) ;
#1091 = CARTESIAN_POINT ( 'NONE',  ( -0.2623718222034988612, -6.245654667075783983, 30.02627829713834018 ) ) ;
#1092 = CARTESIAN_POINT ( 'NONE',  ( 1.035533905932737753, 188.0800000002184902, 4.500000000000000888 ) ) ;
#1093 = CARTESIAN_POINT ( 'NONE',  ( 4.322356511625632614, 7.650514973136570696, 31.00000000000000000 ) ) ;
#1094 = CARTESIAN_POINT ( 'NONE',  ( -0.06647456835015956578, 227.6089819833846093, 5.110108522575333545 ) ) ;
#1095 = FACE_BOUND ( 'NONE', #9024, .T. ) ;
#1096 = CARTESIAN_POINT ( 'NONE',  ( -2.066987299999999195, -0.8561741729129467293, 1.500000001092474777 ) ) ;
#1097 = DIRECTION ( 'NONE',  ( -1.000000000000000000, 0.000000000000000000, 0.000000000000000000 ) ) ;
#1098 = ORIENTED_EDGE ( 'NONE', *, *, #5480, .T. ) ;
#1099 = CARTESIAN_POINT ( 'NONE',  ( -0.8561741729129471734, 187.9999999989075263, 9.066987300000000971 ) ) ;
#1100 = B_SPLINE_CURVE_WITH_KNOTS ( 'NONE', 3,
 ( #15536, #11940, #1046, #5909, #10445, #15299, #4401, #14090, #3200, #89, #15692, #249, #5109, #14813, #9962, #14737, #3898, #10831 ),
 .UNSPECIFIED., .F., .F.,
 ( 4, 2, 2, 2, 2, 2, 2, 2, 4 ),
 ( 0.003131486019301971645, 0.003522824630466680519, 0.003914163241631389394, 0.004305501852796097401, 0.004696840463960806275, 0.005088179075125515149, 0.005479517686290224024, 0.005870856297454932898, 0.006262194908619641773 ),
 .UNSPECIFIED. ) ;
#1101 = CARTESIAN_POINT ( 'NONE',  ( 2.066987300000000083, 187.3999999989075320, 7.856174172912946396 ) ) ;
#1102 = CARTESIAN_POINT ( 'NONE',  ( 13.50000000000000000, 0.000000000000000000, 1.999999999999998668 ) ) ;
#1103 = ORIENTED_EDGE ( 'NONE', *, *, #7106, .F. ) ;
#1104 = AXIS2_PLACEMENT_3D ( 'NONE', #3980, #8858, #13769 ) ;
#1105 = DIRECTION ( 'NONE',  ( 0.000000000000000000, 0.000000000000000000, 1.000000000000000000 ) ) ;
#1106 = CARTESIAN_POINT ( 'NONE',  ( 0.9735954530127236550, -6.173909381473960956, 24.76281793585244628 ) ) ;
#1107 = CARTESIAN_POINT ( 'NONE',  ( 5.999999999999999112, 229.2449477060184222, 9.834870838912449287 ) ) ;
#1108 = CARTESIAN_POINT ( 'NONE',  ( 1.461580736456472573, 188.1499999989075036, 8.461580736456474128 ) ) ;
#1109 = CARTESIAN_POINT ( 'NONE',  ( 2.848235266350879868, 5.281699484015724089, 18.61397738943081848 ) ) ;
#1110 = CARTESIAN_POINT ( 'NONE',  ( -2.500000000000000444, 1.035533905932737753, 0.9500000021849498433 ) ) ;
#1111 = CARTESIAN_POINT ( 'NONE',  ( -0.6156307853269342711, -5.969051238897256972, 31.79870573410679313 ) ) ;
#1112 = B_SPLINE_CURVE_WITH_KNOTS ( 'NONE', 3,
 ( #10937, #12359, #3768, #11248, #11013, #7669, #35, #114, #4901, #1455, #8798, #9830, #7361, #13551, #2660, #9986, #7513, #12280 ),
 .UNSPECIFIED., .F., .F.,
 ( 4, 2, 2, 2, 2, 2, 2, 2, 4 ),
 ( 0.003131486019301987257, 0.003522824630466693963, 0.003914163241631400669, 0.004305501852796107809, 0.004696840463960814081, 0.005088179075125520354, 0.005479517686290227493, 0.005870856297454934633, 0.006262194908619640905 ),
 .UNSPECIFIED. ) ;
#1113 = DIRECTION ( 'NONE',  ( 2.168404344970946942E-15, -1.000000000000000000, -0.000000000000000000 ) ) ;
#1114 = CARTESIAN_POINT ( 'NONE',  ( 0.5039005892421511978, -6.230833003620539046, 30.12636388911297658 ) ) ;
#1115 = DIRECTION ( 'NONE',  ( 0.000000000000000000, 0.000000000000000000, 1.000000000000000000 ) ) ;
#1116 = CARTESIAN_POINT ( 'NONE',  ( -5.317509234263960494, 2.779225709350992890, 30.86935038651144936 ) ) ;
#1117 = ORIENTED_EDGE ( 'NONE', *, *, #6253, .T. ) ;
#1118 = ORIENTED_EDGE ( 'NONE', *, *, #11482, .T. ) ;
#1119 = VERTEX_POINT ( 'NONE', #5492 ) ;
#1120 = CARTESIAN_POINT ( 'NONE',  ( 1.353717517954364224E-13, -6.250000000000000888, 17.99999999999998934 ) ) ;
#1121 = VERTEX_POINT ( 'NONE', #10336 ) ;
#1122 = CARTESIAN_POINT ( 'NONE',  ( -1.265664690411614835E-16, 2.066987299999999639, 1.050000001092474822 ) ) ;
#1123 = CARTESIAN_POINT ( 'NONE',  ( -5.726307184802615247, -2.506131700382550065, 12.30026515017674882 ) ) ;
#1124 = CARTESIAN_POINT ( 'NONE',  ( 4.286401442266544848, -4.198423832313181059, 11.49999999999998224 ) ) ;
#1125 = CARTESIAN_POINT ( 'NONE',  ( 1.461580736456472795, 188.5499999989075093, 5.538419263543527649 ) ) ;
#1126 = CARTESIAN_POINT ( 'NONE',  ( -1.767766952966369098, 1.767766952966369098, 0.006999999978150502240 ) ) ;
#1127 = EDGE_CURVE ( 'NONE', #9974, #8460, #9583, .T. ) ;
#1128 = CARTESIAN_POINT ( 'NONE',  ( 2.897581130414634077E-17, 22.00000000000000000, 11.25000000000000355 ) ) ;
#1129 = CARTESIAN_POINT ( 'NONE',  ( -1.461580736456472351, -1.461580736456473018, -2.649999998907525356 ) ) ;
#1130 = FACE_OUTER_BOUND ( 'NONE', #3700, .T. ) ;
#1131 = CARTESIAN_POINT ( 'NONE',  ( 0.4902782441471901231, 226.3376063806459513, 4.523301387120397088 ) ) ;
#1132 = CARTESIAN_POINT ( 'NONE',  ( 5.558508435838189321, 2.857531096718932684, 5.132341256341690361 ) ) ;
#1133 = VERTEX_POINT ( 'NONE', #11682 ) ;
#1134 = ORIENTED_EDGE ( 'NONE', *, *, #3829, .F. ) ;
#1135 = CARTESIAN_POINT ( 'NONE',  ( 7.799024015210652472, -1.482594289697024781, 11.49999999999998224 ) ) ;
#1136 = ORIENTED_EDGE ( 'NONE', *, *, #3553, .F. ) ;
#1137 = ORIENTED_EDGE ( 'NONE', *, *, #5238, .T. ) ;
#1138 = CARTESIAN_POINT ( 'NONE',  ( 0.8738239080080443255, 6.188820299975592576, 31.50355795710145657 ) ) ;
#1139 = EDGE_CURVE ( 'NONE', #13047, #4415, #4251, .T. ) ;
#1140 = FACE_BOUND ( 'NONE', #7178, .T. ) ;
#1141 = CARTESIAN_POINT ( 'NONE',  ( -3.312341048453529169, -5.004306261885416163, 25.47398020122239259 ) ) ;
#1142 = CARTESIAN_POINT ( 'NONE',  ( 2.668367453516647281, -5.373994336898124224, 11.63061695532137385 ) ) ;
#1143 = EDGE_CURVE ( 'NONE', #8784, #13466, #6997, .T. ) ;
#1144 = CARTESIAN_POINT ( 'NONE',  ( 3.922288969639628586, 4.542045818322656636, 25.37378430870261781 ) ) ;
#1145 = DIRECTION ( 'NONE',  ( -1.000000000000000000, 0.000000000000000000, 0.000000000000000000 ) ) ;
#1146 = CARTESIAN_POINT ( 'NONE',  ( -2.841519077896198731, -5.566940434249990410, 18.26379616840806008 ) ) ;
#1147 = CARTESIAN_POINT ( 'NONE',  ( 5.903347812666343231, 1.076697810262630783, 30.38602261056917442 ) ) ;
#1148 = CARTESIAN_POINT ( 'NONE',  ( 0.8499999999999896527, -0.3999999999999906408, -2.750000000000010658 ) ) ;
#1149 = DIRECTION ( 'NONE',  ( 1.000000000000000000, 0.000000000000000000, 0.000000000000000000 ) ) ;
#1150 = CARTESIAN_POINT ( 'NONE',  ( -2.500000000000000444, 188.2499999978150242, 5.964466094067261359 ) ) ;
#1151 = CARTESIAN_POINT ( 'NONE',  ( 2.734462269239809729, 226.8914732116195125, 6.155466831691636109 ) ) ;
#1152 = DIRECTION ( 'NONE',  ( 1.000000000000000000, 0.000000000000000000, 0.000000000000000000 ) ) ;
#1153 = CARTESIAN_POINT ( 'NONE',  ( -5.558508435838179551, -2.857531096718951336, 31.00000000000000000 ) ) ;
#1154 = ORIENTED_EDGE ( 'NONE', *, *, #15555, .T. ) ;
#1155 = CARTESIAN_POINT ( 'NONE',  ( -4.435347140101170815, 4.403429997944372509, 17.99999999999998934 ) ) ;
#1156 = CARTESIAN_POINT ( 'NONE',  ( -9.750000000000003553, 22.00000000000000000, 1.499999999999965583 ) ) ;
#1158 = EDGE_LOOP ( 'NONE', ( #4293, #1590, #2533, #13794 ) ) ;
#1157 = DIRECTION ( 'NONE',  ( 0.000000000000000000, 0.000000000000000000, 1.000000000000000000 ) ) ;
#1159 = CARTESIAN_POINT ( 'NONE',  ( 3.253823204785200485, -5.337590213880453405, 31.87305891554300530 ) ) ;
#1160 = DIRECTION ( 'NONE',  ( 0.000000000000000000, 0.000000000000000000, -1.000000000000000000 ) ) ;
#1161 = VERTEX_POINT ( 'NONE', #15348 ) ;
#1162 = CARTESIAN_POINT ( 'NONE',  ( 4.153440676704287071, 4.671190581744593118, 23.70045537531157720 ) ) ;
#1163 = CARTESIAN_POINT ( 'NONE',  ( 2.066987300000000083, -0.8561741729129449530, 0.2000000010924747329 ) ) ;
#1164 = CARTESIAN_POINT ( 'NONE',  ( -1.569056679521910747, 226.4669167303270285, 4.904463601914050841 ) ) ;
#1165 =( NAMED_UNIT ( * ) PLANE_ANGLE_UNIT ( ) SI_UNIT ( $, .RADIAN. ) );
#1166 = EDGE_CURVE ( 'NONE', #1681, #6851, #4445, .T. ) ;
#1167 = CARTESIAN_POINT ( 'NONE',  ( -5.648794263291763151, 2.676232015153579447, 12.11441947245483064 ) ) ;
#1168 = CARTESIAN_POINT ( 'NONE',  ( 2.500000000000000444, 187.9800000002184959, 5.964466094067262247 ) ) ;
#1169 = CARTESIAN_POINT ( 'NONE',  ( 6.768587589771821120E-14, -6.250000000000000888, 11.49999999999998224 ) ) ;
#1170 = CARTESIAN_POINT ( 'NONE',  ( 1.986575337946455022, 228.3035988107396292, 7.116201538324070874 ) ) ;
#1171 = CARTESIAN_POINT ( 'NONE',  ( -2.066987299999999639, 0.000000000000000000, -0.1499999989075253282 ) ) ;
#1172 = CARTESIAN_POINT ( 'NONE',  ( 0.6156307853269756825, 5.969051238897252532, 31.79870573410680024 ) ) ;
#1173 = VECTOR ( 'NONE', #15159, 1000.000000000000114 ) ;
#1174 = ORIENTED_EDGE ( 'NONE', *, *, #15351, .F. ) ;
#1175 = CARTESIAN_POINT ( 'NONE',  ( -2.066987300000000971, 187.8499999989074922, 7.000000000000000000 ) ) ;
#1176 = CARTESIAN_POINT ( 'NONE',  ( -4.811147140404425926E-16, 185.6499999989075320, 9.066987300000000971 ) ) ;
#1177 = CARTESIAN_POINT ( 'NONE',  ( -4.070863287254119278, -4.743975846881772540, 12.37305891554299286 ) ) ;
#1178 = VERTEX_POINT ( 'NONE', #15425 ) ;
#1179 = DIRECTION ( 'NONE',  ( -0.000000000000000000, -1.000000000000000000, -0.000000000000000000 ) ) ;
#1180 = DIRECTION ( 'NONE',  ( -0.000000000000000000, 1.000000000000000000, -0.000000000000000000 ) ) ;
#1181 = CARTESIAN_POINT ( 'NONE',  ( 5.616089948629732653, -2.743103014345535939, 31.50436969680151833 ) ) ;
#1182 = DIRECTION ( 'NONE',  ( 0.9510565162951500895, 0.3090169943749582204, 0.000000000000000000 ) ) ;
#1183 = CARTESIAN_POINT ( 'NONE',  ( -0.5030929395819625505, -6.230885867001150658, 10.62600319116547887 ) ) ;
#1184 = CARTESIAN_POINT ( 'NONE',  ( 2.668367453516689025, -5.373994336898102908, 30.86935038651144936 ) ) ;
#1185 = CARTESIAN_POINT ( 'NONE',  ( 1.214065608363191773, 189.0732342899627554, 9.931872992141947520 ) ) ;
#1186 = LINE ( 'NONE', #11515, #5034 ) ;
#1187 = CARTESIAN_POINT ( 'NONE',  ( 5.665824935993619249, -1.978765057080893008, 31.99995053646223653 ) ) ;
#1188 = CARTESIAN_POINT ( 'NONE',  ( -4.416678568553713546, 4.422441866694247103, 30.73763026556126121 ) ) ;
#1189 = CARTESIAN_POINT ( 'NONE',  ( 5.620786884546266293, 2.102685372472950398, 4.026414045633067929 ) ) ;
#1190 = CARTESIAN_POINT ( 'NONE',  ( 2.500000000000000444, 187.2500000000000000, 5.964466094067262247 ) ) ;
#1191 = ORIENTED_EDGE ( 'NONE', *, *, #15384, .T. ) ;
#1192 = ORIENTED_EDGE ( 'NONE', *, *, #7499, .T. ) ;
#1193 = ADVANCED_BREP_SHAPE_REPRESENTATION ( '', ( #15484, #14201 ), #5333 ) ;
#1194 = ORIENTED_EDGE ( 'NONE', *, *, #6676, .T. ) ;
#1195 = CYLINDRICAL_SURFACE ( 'NONE', #1471, 1.000000000000000666 ) ;
#1196 = ORIENTED_EDGE ( 'NONE', *, *, #14425, .T. ) ;
#1197 = CARTESIAN_POINT ( 'NONE',  ( -1.767766952966369098, 1.767766952966369098, -3.099999997815050090 ) ) ;
#1198 = CARTESIAN_POINT ( 'NONE',  ( 0.2624013748573172378, 5.995472630654518298, 4.026285596910829767 ) ) ;
#1199 = FACE_OUTER_BOUND ( 'NONE', #10909, .T. ) ;
#1200 = CARTESIAN_POINT ( 'NONE',  ( 0.000000000000000000, 2.000000000000000000, 0.000000000000000000 ) ) ;
#1201 = CARTESIAN_POINT ( 'NONE',  ( -0.8561741729129467293, 186.5999999989075206, 9.066987299999999195 ) ) ;
#1202 = CARTESIAN_POINT ( 'NONE',  ( 1.035533905932739085, -2.500000000000000000, 1.949999999999999956 ) ) ;
#1203 = AXIS2_PLACEMENT_3D ( 'NONE', #11068, #5988, #10992 ) ;
#1204 = CARTESIAN_POINT ( 'NONE',  ( -5.665308849928837986, 1.980336949702462990, 31.99992002356261267 ) ) ;
#1205 = CONTEXT_DEPENDENT_SHAPE_REPRESENTATION ( #11072, #11601 ) ;
#1206 = CARTESIAN_POINT ( 'NONE',  ( 1.461580736456472573, 1.461580736456472795, -1.449999998907525178 ) ) ;
#1207 = DIRECTION ( 'NONE',  ( 0.5877852522924802425, -0.8090169943749422332, 0.000000000000000000 ) ) ;
#1208 = CARTESIAN_POINT ( 'NONE',  ( -1.586193948774629714, 228.1096603596491832, 9.740555404025270647 ) ) ;
#1209 = CARTESIAN_POINT ( 'NONE',  ( 12.50000000000000533, 1.530808498934192113E-15, 2.000000000000001776 ) ) ;
#1210 = ORIENTED_EDGE ( 'NONE', *, *, #2448, .T. ) ;
#1211 = ORIENTED_EDGE ( 'NONE', *, *, #8936, .F. ) ;
#1212 = LINE ( 'NONE', #9499, #3758 ) ;
#1213 = CIRCLE ( 'NONE', #1462, 3.000000000000000000 ) ;
#1214 = VERTEX_POINT ( 'NONE', #12948 ) ;
#1215 = ORIENTED_EDGE ( 'NONE', *, *, #13936, .T. ) ;
#1216 = EDGE_CURVE ( 'NONE', #4645, #660, #6788, .T. ) ;
#1217 = CARTESIAN_POINT ( 'NONE',  ( -6.172552660730963758, 0.9821660343539665439, 24.76379616840807074 ) ) ;
#1218 = CIRCLE ( 'NONE', #5792, 1.499999999999999556 ) ;
#1219 = DIRECTION ( 'NONE',  ( 0.5000000000000001110, 0.8660254037844385966, 0.000000000000000000 ) ) ;
#1220 = CARTESIAN_POINT ( 'NONE',  ( -2.668367453516813814, -5.373994336898041624, 24.49999999999999289 ) ) ;
#1221 = CARTESIAN_POINT ( 'NONE',  ( -6.142908455506939980, -1.155755562476076692, 31.61517780375841369 ) ) ;
#1222 = CARTESIAN_POINT ( 'NONE',  ( 2.996417732210474583, -5.485687819086957795, 23.88603820591927729 ) ) ;
#1223 = CARTESIAN_POINT ( 'NONE',  ( 0.000000000000000000, 0.000000000000000000, 2.500000000000000000 ) ) ;
#1224 = CARTESIAN_POINT ( 'NONE',  ( -3.255013540813683992, -5.336859797930807225, 18.87381964045070504 ) ) ;
#1225 =( BOUNDED_CURVE ( )  B_SPLINE_CURVE ( 2, ( #7222, #1312, #3703, #5945, #2434, #10948, #6026, #13171, #4990 ),
 .UNSPECIFIED., .F., .F. ) 
 B_SPLINE_CURVE_WITH_KNOTS ( ( 3, 2, 2, 2, 3 ),
 ( 0.6428571428571429047, 0.6607142857142856984, 0.6785714285714286031, 0.6964285714285713969, 0.7142857142857143016 ),
 .UNSPECIFIED. ) 
 CURVE ( )  GEOMETRIC_REPRESENTATION_ITEM ( )  RATIONAL_B_SPLINE_CURVE ( ( 1.000000000000000000, 0.9238795325112867385, 1.000000000000000000, 0.9238795325112867385, 1.000000000000000000, 0.9238795325112867385, 1.000000000000000000, 0.9238795325112867385, 1.000000000000000000 ) ) 
 REPRESENTATION_ITEM ( '' )  );
#1226 = DIRECTION ( 'NONE',  ( 0.000000000000000000, 0.000000000000000000, 1.000000000000000000 ) ) ;
#1227 = CARTESIAN_POINT ( 'NONE',  ( -1.767766952966369320, 188.2999999999999829, 5.232233047033630235 ) ) ;
#1228 = DIRECTION ( 'NONE',  ( -1.000000000000000000, 0.000000000000000000, -3.491481338843133355E-15 ) ) ;
#1229 = VECTOR ( 'NONE', #2016, 1000.000000000000000 ) ;
#1230 = CARTESIAN_POINT ( 'NONE',  ( 1.035533905932737753, 188.0499999978150640, 4.500000000000000888 ) ) ;
#1231 = CARTESIAN_POINT ( 'NONE',  ( 1.978507955918972439, 228.0159604248740663, 9.465015589616863068 ) ) ;
#1232 = CARTESIAN_POINT ( 'NONE',  ( 5.558508435838260375, -2.857531096718793240, 11.49999999999998224 ) ) ;
#1233 = B_SPLINE_CURVE_WITH_KNOTS ( 'NONE', 3,
 ( #13622, #9902, #1686, #2656, #11242, #3997, #2735, #7587, #14990, #4081, #12434, #8952, #344, #5206, #10059, #7664, #13783, #3047 ),
 .UNSPECIFIED., .F., .F.,
 ( 4, 2, 2, 2, 2, 2, 2, 2, 4 ),
 ( 0.000000000000000000, 0.0003914904498596246838, 0.0007829808997192493677, 0.001174471349578873943, 0.001565961799438498735, 0.001957452249298123528, 0.002348942699157747886, 0.002740433149017372678, 0.003131923598876997471 ),
 .UNSPECIFIED. ) ;
#1234 = ADVANCED_FACE ( 'NONE', ( #11755 ), #14216, .F. ) ;
#1235 = CARTESIAN_POINT ( 'NONE',  ( -1.760080037233190620, 188.9999999985105887, 5.215340696719847458 ) ) ;
#1236 = ORIENTED_EDGE ( 'NONE', *, *, #9801, .T. ) ;
#1237 = CARTESIAN_POINT ( 'NONE',  ( -5.409007216690679520, 2.598315788643733804, 12.11442521571935949 ) ) ;
#1238 = CARTESIAN_POINT ( 'NONE',  ( 6.768587589771821120E-14, -6.000000000000000888, 12.49999999999998401 ) ) ;
#1239 = CARTESIAN_POINT ( 'NONE',  ( 5.330189595673696878, 2.755293208590127385, 24.76382603205595956 ) ) ;
#1240 = CARTESIAN_POINT ( 'NONE',  ( 0.06960442597363748762, -0.3999999999999923617, 2.548071207443342701 ) ) ;
#1241 = FACE_OUTER_BOUND ( 'NONE', #4971, .T. ) ;
#1242 = EDGE_CURVE ( 'NONE', #5900, #7812, #3452, .T. ) ;
#1243 = CARTESIAN_POINT ( 'NONE',  ( 3.158296126777660362, 5.394094919772187247, 23.70112161576660981 ) ) ;
#1244 = CARTESIAN_POINT ( 'NONE',  ( -0.8561741729129458411, -2.066987299999999195, -0.7999999989075252671 ) ) ;
#1245 = CARTESIAN_POINT ( 'NONE',  ( -2.817313151351372724, 5.579000502529339656, 24.36765874365829987 ) ) ;
#1246 = CARTESIAN_POINT ( 'NONE',  ( 2.082642335314403343E-14, -6.250000000000000888, 32.00000000000000000 ) ) ;
#1247 = CARTESIAN_POINT ( 'NONE',  ( 1.767766952966369320, 184.0999999999999943, 5.232233047033630235 ) ) ;
#1248 = DIRECTION ( 'NONE',  ( 0.000000000000000000, 0.000000000000000000, 1.000000000000000000 ) ) ;
#1249 = CARTESIAN_POINT ( 'NONE',  ( 0.5151998000674417044, 228.8897689535086784, 8.809094343595948118 ) ) ;
#1250 = CARTESIAN_POINT ( 'NONE',  ( 1.461580736456472573, 1.461580736456472795, 0.3500000010924749216 ) ) ;
#1251 = CARTESIAN_POINT ( 'NONE',  ( 0.9739805876848109945, 5.920636045238163447, 31.26171386814423414 ) ) ;
#1252 = VERTEX_POINT ( 'NONE', #5319 ) ;
#1253 = CARTESIAN_POINT ( 'NONE',  ( -1.456896669277396583E-16, 188.4499999989075150, 4.933012699999999029 ) ) ;
#1254 = CARTESIAN_POINT ( 'NONE',  ( 1.461580736456472573, 187.3499999989074922, 8.461580736456474128 ) ) ;
#1255 = DIRECTION ( 'NONE',  ( 0.000000000000000000, 0.000000000000000000, 1.000000000000000000 ) ) ;
#1256 = ORIENTED_EDGE ( 'NONE', *, *, #12219, .T. ) ;
#1257 = ADVANCED_FACE ( 'NONE', ( #11272 ), #7034, .T. ) ;
#1258 = CARTESIAN_POINT ( 'NONE',  ( 0.000000000000000000, 0.000000000000000000, 0.000000000000000000 ) ) ;
#1259 = VECTOR ( 'NONE', #15235, 1000.000000000000227 ) ;
#1260 = CARTESIAN_POINT ( 'NONE',  ( 1.530808498934191324E-15, 184.0000000000000000, 12.49999999999999822 ) ) ;
#1261 = DIRECTION ( 'NONE',  ( 0.8090169943749506709, -0.5877852522924689183, 0.000000000000000000 ) ) ;
#1262 = CARTESIAN_POINT ( 'NONE',  ( -1.474837674502392115, 189.0000000000000568, 9.021725798137643082 ) ) ;
#1263 = CARTESIAN_POINT ( 'NONE',  ( 4.142173849413661735, 4.341773579105486114, 18.61519382448850024 ) ) ;
#1264 = CARTESIAN_POINT ( 'NONE',  ( -2.500000000000000444, 1.035533905932737753, -3.049999997815050268 ) ) ;
#1265 = CARTESIAN_POINT ( 'NONE',  ( -2.897581130414634077E-17, 9.750000000000003553, 2.000000000000001776 ) ) ;
#1266 = CARTESIAN_POINT ( 'NONE',  ( 5.935543223013869607, -0.8771126767605967878, 11.49999999999998224 ) ) ;
#1267 = CARTESIAN_POINT ( 'NONE',  ( -4.070863287254157470, 4.743975846881738789, 30.12694108445699825 ) ) ;
#1268 = CARTESIAN_POINT ( 'NONE',  ( -6.176542424588110869, 0.9554180641286129649, 11.49999999999998224 ) ) ;
#1269 = CARTESIAN_POINT ( 'NONE',  ( -5.666074146198023520, 1.978051345703084385, 29.99995067926688819 ) ) ;
#1270 = ORIENTED_EDGE ( 'NONE', *, *, #12295, .F. ) ;
#1271 = AXIS2_PLACEMENT_3D ( 'NONE', #2509, #1382, #9760 ) ;
#1272 = VERTEX_POINT ( 'NONE', #10086 ) ;
#1273 = ORIENTED_EDGE ( 'NONE', *, *, #3458, .F. ) ;
#1274 = EDGE_CURVE ( 'NONE', #2475, #11794, #294, .T. ) ;
#1275 = CARTESIAN_POINT ( 'NONE',  ( -5.621278735166150398, -2.101423246382678744, 25.47408052783099919 ) ) ;
#1276 = B_SPLINE_CURVE_WITH_KNOTS ( 'NONE', 3,
 ( #2879, #12420, #7725, #4143, #9093, #13690, #1753, #3903, #8778, #2799, #1830, #3034, #7887, #5354, #10200, #15051, #6704, #1518 ),
 .UNSPECIFIED., .F., .F.,
 ( 4, 2, 2, 2, 2, 2, 2, 2, 4 ),
 ( 0.003131918686235972155, 0.003523310662250262858, 0.003914702638264553128, 0.004306094614278843831, 0.004697486590293134534, 0.005088878566307425237, 0.005480270542321715940, 0.005871662518336006643, 0.006263054494350297347 ),
 .UNSPECIFIED. ) ;
#1277 = ORIENTED_EDGE ( 'NONE', *, *, #7956, .F. ) ;
#1278 = CARTESIAN_POINT ( 'NONE',  ( 2.500000000000000000, 3.061616997868383141E-16, -2.599999997815050534 ) ) ;
#1279 = CARTESIAN_POINT ( 'NONE',  ( -5.558508435838157347, -2.857531096718993080, 11.49999999999998224 ) ) ;
#1280 = CARTESIAN_POINT ( 'NONE',  ( -7.490007020835699691, -2.433650805992386701, 31.00000000000000000 ) ) ;
#1281 = CARTESIAN_POINT ( 'NONE',  ( -5.421010862427522170E-16, 186.6499999989075320, 9.066987300000000971 ) ) ;
#1282 = CARTESIAN_POINT ( 'NONE',  ( 2.500000000000000444, 1.035533905932737975, 2.149999999999999911 ) ) ;
#1283 = CARTESIAN_POINT ( 'NONE',  ( -5.935543223013858949, 0.8771126767606858277, 31.13236078583911137 ) ) ;
#1284 = ITEM_DEFINED_TRANSFORMATION ( 'NONE', 'NONE', #3303,  #14201 ) ;
#1285 = CARTESIAN_POINT ( 'NONE',  ( -5.726307184802553962, -2.506131700382691285, 25.30026515017674882 ) ) ;
#1286 = CARTESIAN_POINT ( 'NONE',  ( 1.461580736456473018, -1.461580736456472573, -2.449999998907525622 ) ) ;
#1287 = CARTESIAN_POINT ( 'NONE',  ( 4.435347140101058905, -4.403429997944484420, 31.00000000000000000 ) ) ;
#1288 = CARTESIAN_POINT ( 'NONE',  ( -3.000008639299222235, 227.3051114066062155, 7.373492455173472848 ) ) ;
#1289 = CARTESIAN_POINT ( 'NONE',  ( 5.649200442566134406, 2.675373855294195913, 5.615601928929211617 ) ) ;
#1290 = VERTEX_POINT ( 'NONE', #6516 ) ;
#1291 = ORIENTED_EDGE ( 'NONE', *, *, #10850, .F. ) ;
#1292 = ORIENTED_EDGE ( 'NONE', *, *, #15126, .F. ) ;
#1293 = ORIENTED_EDGE ( 'NONE', *, *, #3939, .T. ) ;
#1294 = DIRECTION ( 'NONE',  ( 0.000000000000000000, 0.000000000000000000, 1.000000000000000000 ) ) ;
#1295 = CARTESIAN_POINT ( 'NONE',  ( 0.9740856415300854776, -6.173834621338593287, 4.738526530555332350 ) ) ;
#1296 = CARTESIAN_POINT ( 'NONE',  ( -6.105861027178969280, 1.337741388556907385, 31.79954462468843346 ) ) ;
#1297 = CARTESIAN_POINT ( 'NONE',  ( 1.000079958708202321, 5.916066267613690144, 11.63152738882033788 ) ) ;
#1298 = CARTESIAN_POINT ( 'NONE',  ( 7.347880794884119736E-16, -6.250000000000000888, 4.000000000000004441 ) ) ;
#1299 = CARTESIAN_POINT ( 'NONE',  ( 5.317509234264001350, -2.779225709350912954, 11.49999999999998224 ) ) ;
#1300 = CARTESIAN_POINT ( 'NONE',  ( 0.9740807849837530563, -5.920620690450666856, 17.73850119700669481 ) ) ;
#1301 = CARTESIAN_POINT ( 'NONE',  ( 0.000000000000000000, 184.0000000000000000, 7.000000000000000000 ) ) ;
#1302 = CARTESIAN_POINT ( 'NONE',  ( 0.000000000000000000, 142.0000000000000284, 0.000000000000000000 ) ) ;
#1303 = CARTESIAN_POINT ( 'NONE',  ( -4.743384504624081899E-17, 187.2999999978150356, 4.500000000000000000 ) ) ;
#1304 = B_SPLINE_CURVE_WITH_KNOTS ( 'NONE', 3,
 ( #10279, #6478, #11312, #5359, #489, #7967, #5279, #8863, #7654, #4148, #10050, #13926, #14898, #4227, #13847, #3037, #566, #2960 ),
 .UNSPECIFIED., .F., .F.,
 ( 4, 2, 2, 2, 2, 2, 2, 2, 4 ),
 ( 0.000000000000000000, 0.0003914898357794971157, 0.0007829796715589942314, 0.001174469507338491347, 0.001565959343117988463, 0.001957449178897485362, 0.002348939014676982694, 0.002740428850456480027, 0.003131918686235976926 ),
 .UNSPECIFIED. ) ;
#1305 = CARTESIAN_POINT ( 'NONE',  ( 2.053141855112443626, 226.5855735425530497, 5.254201149538955562 ) ) ;
#1306 = DIRECTION ( 'NONE',  ( -0.000000000000000000, 1.000000000000000000, -0.000000000000000000 ) ) ;
#1307 =( REPRESENTATION_RELATIONSHIP ('NONE','NONE', #11191, #9569 ) REPRESENTATION_RELATIONSHIP_WITH_TRANSFORMATION ( #10046 )SHAPE_REPRESENTATION_RELATIONSHIP( ) );
#1308 = CARTESIAN_POINT ( 'NONE',  ( -2.990615845299959386, 189.8642828410552568, 7.611177514557324386 ) ) ;
#1309 = EDGE_LOOP ( 'NONE', ( #10925, #13095 ) ) ;
#1310 = CARTESIAN_POINT ( 'NONE',  ( 0.000000000000000000, 0.000000000000000000, 36.00000000000000711 ) ) ;
#1311 = CARTESIAN_POINT ( 'NONE',  ( -0.5031281619707089758, -5.980084330432673845, 10.62602272744524079 ) ) ;
#1312 = CARTESIAN_POINT ( 'NONE',  ( -2.500000000000001776, 187.6500000000000057, 8.035533905932737753 ) ) ;
#1313 = CARTESIAN_POINT ( 'NONE',  ( 4.153440676704482470, -4.671190581744419035, 31.79954462468844056 ) ) ;
#1314 = CIRCLE ( 'NONE', #7917, 6.000000000000000000 ) ;
#1315 = CARTESIAN_POINT ( 'NONE',  ( -5.000000000000000000, 0.000000000000000000, 52.97056274847714263 ) ) ;
#1316 =( BOUNDED_CURVE ( )  B_SPLINE_CURVE ( 2, ( #3770, #7290, #8570, #6015, #13628, #12126, #1227, #6178, #2507 ),
 .UNSPECIFIED., .F., .F. ) 
 B_SPLINE_CURVE_WITH_KNOTS ( ( 3, 2, 2, 2, 3 ),
 ( 0.7142857142857143016, 0.7321428571428570953, 0.7500000000000000000, 0.7678571428571429047, 0.7857142857142856984 ),
 .UNSPECIFIED. ) 
 CURVE ( )  GEOMETRIC_REPRESENTATION_ITEM ( )  RATIONAL_B_SPLINE_CURVE ( ( 1.000000000000000000, 0.9238795325112867385, 1.000000000000000000, 0.9238795325112867385, 1.000000000000000000, 0.9238795325112867385, 1.000000000000000000, 0.9238795325112867385, 1.000000000000000000 ) ) 
 REPRESENTATION_ITEM ( '' )  );
#1317 = CARTESIAN_POINT ( 'NONE',  ( -3.312341048453488312, 5.004306261885441032, 10.52601979877758964 ) ) ;
#1318 = CARTESIAN_POINT ( 'NONE',  ( 2.066987299999999639, 2.531329380823229670E-16, 1.850000001092474866 ) ) ;
#1319 = LINE ( 'NONE', #1789, #9211 ) ;
#1320 = ADVANCED_FACE ( 'NONE', ( #2764, #8667 ), #14937, .F. ) ;
#1321 = LINE ( 'NONE', #6197, #2164 ) ;
#1322 = CARTESIAN_POINT ( 'NONE',  ( 1.035533905932738197, 186.9800000002184674, 9.500000000000003553 ) ) ;
#1323 = FACE_BOUND ( 'NONE', #11390, .T. ) ;
#1324 = EDGE_CURVE ( 'NONE', #3143, #14086, #11349, .T. ) ;
#1325 = CARTESIAN_POINT ( 'NONE',  ( 1.159630251547017377, 228.7900363578050928, 8.521060918829135744 ) ) ;
#1326 = CARTESIAN_POINT ( 'NONE',  ( -0.8561741729129455081, 2.066987299999999639, -2.699999998907525622 ) ) ;
#1327 = VECTOR ( 'NONE', #1359, 1000.000000000000000 ) ;
#1328 = CARTESIAN_POINT ( 'NONE',  ( 5.858736126997162508, 2.179962889276984228, 17.02640428276697904 ) ) ;
#1329 = ADVANCED_FACE ( 'NONE', ( #15019 ), #4027, .T. ) ;
#1330 = ORIENTED_EDGE ( 'NONE', *, *, #2807, .T. ) ;
#1331 = CARTESIAN_POINT ( 'NONE',  ( 1.461580736456473240, 186.7499999989075263, 5.538419263543526760 ) ) ;
#1332 = CARTESIAN_POINT ( 'NONE',  ( -0.8561741729129469514, 184.7999999989075093, 9.066987300000000971 ) ) ;
#1333 = CARTESIAN_POINT ( 'NONE',  ( 5.486982057989233219, 2.429327048029787051, 23.70068193741825269 ) ) ;
#1335 = ORIENTED_EDGE ( 'NONE', *, *, #5940, .T. ) ;
#1334 = CARTESIAN_POINT ( 'NONE',  ( 4.141923667210567039, -4.342011609040540954, 25.11561732698605098 ) ) ;
#1336 = CARTESIAN_POINT ( 'NONE',  ( -4.267992336621275307, -4.217442018459924391, 24.23805675996853992 ) ) ;
#1337 = CARTESIAN_POINT ( 'NONE',  ( 0.1306394121201409075, -6.249999999999997335, 23.50000000000000000 ) ) ;
#1338 = CIRCLE ( 'NONE', #13277, 1.500000000000000000 ) ;
#1339 = CARTESIAN_POINT ( 'NONE',  ( 6.081590040723082957, -1.446205118472983164, 31.87367328635992081 ) ) ;
#1340 = CARTESIAN_POINT ( 'NONE',  ( 5.999999999999999112, 188.6555110544239824, 3.692234042173051289 ) ) ;
#1341 = CARTESIAN_POINT ( 'NONE',  ( -1.000082492230644826, -6.169467968613719044, 11.63152538105391365 ) ) ;
#1342 = CARTESIAN_POINT ( 'NONE',  ( 5.531796221294958293, -2.326749136277022512, 25.37378430870261781 ) ) ;
#1343 = CARTESIAN_POINT ( 'NONE',  ( -2.500000000000000000, 0.000000000000000000, -2.999999997815050889 ) ) ;
#1344 = DIRECTION ( 'NONE',  ( 0.000000000000000000, 0.000000000000000000, 1.000000000000000000 ) ) ;
#1345 = CARTESIAN_POINT ( 'NONE',  ( 5.935543223013868719, -0.8771126767605967878, 11.36938304467859773 ) ) ;
#1346 = CARTESIAN_POINT ( 'NONE',  ( -5.531623157106168698, 2.327208526676430189, 10.62635295315575235 ) ) ;
#1347 = CARTESIAN_POINT ( 'NONE',  ( 9.750000000000003553, 184.0000000000000000, 1.020968533498575461E-13 ) ) ;
#1348 =( BOUNDED_CURVE ( )  B_SPLINE_CURVE ( 2, ( #10407, #14208, #8258, #15500, #4597, #14130, #12939, #9217, #6837 ),
 .UNSPECIFIED., .F., .F. ) 
 B_SPLINE_CURVE_WITH_KNOTS ( ( 3, 2, 2, 2, 3 ),
 ( 0.4285714285714285476, 0.4464285714285714524, 0.4642857142857143016, 0.4821428571428571508, 0.5000000000000000000 ),
 .UNSPECIFIED. ) 
 CURVE ( )  GEOMETRIC_REPRESENTATION_ITEM ( )  RATIONAL_B_SPLINE_CURVE ( ( 1.000000000000000000, 0.9238795325112867385, 1.000000000000000000, 0.9238795325112867385, 1.000000000000000000, 0.9238795325112867385, 1.000000000000000000, 0.9238795325112867385, 1.000000000000000000 ) ) 
 REPRESENTATION_ITEM ( '' )  );
#1349 = CARTESIAN_POINT ( 'NONE',  ( 3.106366801611825768, 5.134708448381389623, 23.62696220972947359 ) ) ;
#1350 = ORIENTED_EDGE ( 'NONE', *, *, #8234, .T. ) ;
#1351 = EDGE_LOOP ( 'NONE', ( #3419, #1134, #3681, #13778, #10714 ) ) ;
#1352 = EDGE_LOOP ( 'NONE', ( #15708, #4672 ) ) ;
#1353 = DIRECTION ( 'NONE',  ( -1.000000000000000000, -6.123233995736766036E-17, 0.000000000000000000 ) ) ;
#1354 = ORIENTED_EDGE ( 'NONE', *, *, #6985, .F. ) ;
#1355 = EDGE_CURVE ( 'NONE', #5666, #5381, #15411, .T. ) ;
#1356 = CARTESIAN_POINT ( 'NONE',  ( -1.461580736456472795, 1.461580736456472795, 0.3500000010924746996 ) ) ;
#1357 = CARTESIAN_POINT ( 'NONE',  ( -6.142908455506926657, -1.155755562476141973, 12.11517780375842790 ) ) ;
#1358 = CARTESIAN_POINT ( 'NONE',  ( 6.176542424588128632, -0.9554180641284775177, 11.49999999999998224 ) ) ;
#1359 = DIRECTION ( 'NONE',  ( 0.5877852522924802425, -0.8090169943749422332, 0.000000000000000000 ) ) ;
#1360 = VECTOR ( 'NONE', #9407, 1000.000000000000000 ) ;
#1361 = CARTESIAN_POINT ( 'NONE',  ( -1.035533905932737753, 2.500000000000000444, 1.550000000000000044 ) ) ;
#1362 = CARTESIAN_POINT ( 'NONE',  ( 5.558508435838229289, -2.857531096718853192, 4.867658743658316745 ) ) ;
#1363 = CONTEXT_DEPENDENT_SHAPE_REPRESENTATION ( #9428, #15428 ) ;
#1364 = DIRECTION ( 'NONE',  ( 0.9510565162951499785, 0.3090169943749582204, 0.000000000000000000 ) ) ;
#1365 = CARTESIAN_POINT ( 'NONE',  ( -0.8561741729129458411, -2.066987299999999195, -0.9999999989075254447 ) ) ;
#1366 = ADVANCED_FACE ( 'NONE', ( #7460, #12303 ), #1401, .F. ) ;
#1367 = CARTESIAN_POINT ( 'NONE',  ( -5.648559266344550522, 2.676764518775886170, 30.38603820591929505 ) ) ;
#1368 = CARTESIAN_POINT ( 'NONE',  ( -2.980755195990519191, 227.3998431049529074, 7.652341518474168325 ) ) ;
#1369 = EDGE_LOOP ( 'NONE', ( #1607, #4828, #4050, #11315 ) ) ;
#1370 = ORIENTED_EDGE ( 'NONE', *, *, #3477, .F. ) ;
#1371 = EDGE_CURVE ( 'NONE', #4873, #14187, #2186, .T. ) ;
#1372 = EDGE_LOOP ( 'NONE', ( #10888, #2354, #4868, #12038 ) ) ;
#1373 = CARTESIAN_POINT ( 'NONE',  ( 5.317509234263979145, -2.779225709350955142, 31.00000000000000000 ) ) ;
#1374 = CARTESIAN_POINT ( 'NONE',  ( 0.6408967124214390854, 189.0000000000000000, 9.420550828545728450 ) ) ;
#1375 = CARTESIAN_POINT ( 'NONE',  ( -5.769755079862245672, -2.405651898699154412, 17.12694108445698760 ) ) ;
#1376 = CARTESIAN_POINT ( 'NONE',  ( -3.736532060718029680, -4.696070028785941375, 18.97377823943292086 ) ) ;
#1377 = CARTESIAN_POINT ( 'NONE',  ( 0.2624013748573880700, 5.995472630654516522, 10.52628559691080845 ) ) ;
#1378 = CARTESIAN_POINT ( 'NONE',  ( 0.000000000000000000, 0.000000000000000000, 2.000000000000001776 ) ) ;
#1379 = DIRECTION ( 'NONE',  ( -0.000000000000000000, -1.000000000000000000, -0.000000000000000000 ) ) ;
#1380 = CARTESIAN_POINT ( 'NONE',  ( -5.770167736194696140, -2.404664418229167655, 5.873673286359928802 ) ) ;
#1381 = CARTESIAN_POINT ( 'NONE',  ( 0.1306497350719363348, -5.999999999999997335, 23.50000000000000000 ) ) ;
#1382 = DIRECTION ( 'NONE',  ( -1.000000000000000000, 0.000000000000000000, -3.491481338843133355E-15 ) ) ;
#1383 = CARTESIAN_POINT ( 'NONE',  ( 1.035533905932737975, 185.7199999975966023, 4.500000000000000888 ) ) ;
#1384 = CARTESIAN_POINT ( 'NONE',  ( -1.673363231402341000, 227.9073979391035891, 5.971950823222174520 ) ) ;
#1385 = CARTESIAN_POINT ( 'NONE',  ( 1.059913075168976260, 226.3867898013274669, 4.668296007112484602 ) ) ;
#1386 = CARTESIAN_POINT ( 'NONE',  ( -0.2831953767659359800, 189.6983146630735177, 10.38325066061015178 ) ) ;
#1387 = ORIENTED_EDGE ( 'NONE', *, *, #10097, .T. ) ;
#1388 = CARTESIAN_POINT ( 'NONE',  ( -3.061616997868391523E-16, 182.0000000000000000, 7.000000000000000000 ) ) ;
#1389 = CARTESIAN_POINT ( 'NONE',  ( -6.176542424588090441, 0.9554180641287483011, 24.36762589283695135 ) ) ;
#1390 = CARTESIAN_POINT ( 'NONE',  ( -1.530808498934191571E-16, 2.500000000000000000, -0.9000000000000002442 ) ) ;
#1391 = DIRECTION ( 'NONE',  ( -0.3090169943749584425, 0.9510565162951498674, 0.000000000000000000 ) ) ;
#1392 = CARTESIAN_POINT ( 'NONE',  ( 0.07962197837297851910, 190.0874091994478761, 4.202769589527710181 ) ) ;
#1393 = DIRECTION ( 'NONE',  ( -1.000000000000000000, 0.000000000000000000, 0.000000000000000000 ) ) ;
#1394 = CARTESIAN_POINT ( 'NONE',  ( -1.461580736456472351, -1.461580736456473018, -2.449999998907525178 ) ) ;
#1395 = CARTESIAN_POINT ( 'NONE',  ( 5.409423237179020738, -2.597448116731011947, 4.384382673013947240 ) ) ;
#1396 = CARTESIAN_POINT ( 'NONE',  ( -7.799024015210601846, -1.482594289697409140, 24.49999999999999289 ) ) ;
#1397 = CARTESIAN_POINT ( 'NONE',  ( -1.035533905932737975, 186.5800000002185470, 4.500000000000000888 ) ) ;
#1398 = DIRECTION ( 'NONE',  ( 0.000000000000000000, -2.775557561562888393E-16, 1.000000000000000000 ) ) ;
#1399 = ADVANCED_FACE ( 'NONE', ( #6747 ), #5475, .F. ) ;
#1400 = CARTESIAN_POINT ( 'NONE',  ( 1.637003574519428017, 228.6312591184326948, 8.062503195461440342 ) ) ;
#1401 = PLANE ( 'NONE',  #12108 ) ;
#1402 = CARTESIAN_POINT ( 'NONE',  ( -2.500000000000000444, 1.035533905932737753, 1.649999999999999911 ) ) ;
#1403 = ORIENTED_EDGE ( 'NONE', *, *, #13029, .F. ) ;
#1404 = DIRECTION ( 'NONE',  ( 0.000000000000000000, 1.000000000000000000, 0.000000000000000000 ) ) ;
#1405 = CARTESIAN_POINT ( 'NONE',  ( 1.767766952966368654, 185.5000000000000000, 8.767766952966368876 ) ) ;
#1406 = CARTESIAN_POINT ( 'NONE',  ( -5.935543223013825198, -0.8771126767608831143, 18.13239388001634467 ) ) ;
#1408 = ORIENTED_EDGE ( 'NONE', *, *, #10506, .F. ) ;
#1407 = CARTESIAN_POINT ( 'NONE',  ( 4.416397290909897855, 4.422724436066440390, 30.73620383159192215 ) ) ;
#1409 = ADVANCED_FACE ( 'NONE', ( #4503, #5705, #527, #5395, #4349, #9206, #7924, #10317, #1794, #12767, #9284, #13968, #15328, #15170, #12928, #9134, #10243, #4269, #10549, #15094, #6591, #676, #5627, #9359, #14044, #3153 ), #13886, .F. ) ;
#1410 = CYLINDRICAL_SURFACE ( 'NONE', #10422, 1.000000000000000888 ) ;
#1411 = CARTESIAN_POINT ( 'NONE',  ( 5.570760634536836342, -2.834026536768180282, 11.76225281721714389 ) ) ;
#1412 = DIRECTION ( 'NONE',  ( 0.9961946980917455452, 2.087662678150794344E-17, -0.08715574274765844343 ) ) ;
#1413 = CARTESIAN_POINT ( 'NONE',  ( 0.6156133477427008227, 6.220296490279941359, 12.29872387345513474 ) ) ;
#1414 = CARTESIAN_POINT ( 'NONE',  ( -0.1306070469492700281, -6.250000000000000888, 10.49999999999998579 ) ) ;
#1415 = CARTESIAN_POINT ( 'NONE',  ( 5.375886393124466700, -2.665038680141120331, 25.00439760644211873 ) ) ;
#1416 = DIRECTION ( 'NONE',  ( 0.000000000000000000, 0.000000000000000000, 1.000000000000000000 ) ) ;
#1417 = LINE ( 'NONE', #14557, #14169 ) ;
#1418 = VECTOR ( 'NONE', #14560, 1000.000000000000000 ) ;
#1419 = CARTESIAN_POINT ( 'NONE',  ( 2.668367453516707233, -5.373994336898093138, 5.000000000000004441 ) ) ;
#1420 = CARTESIAN_POINT ( 'NONE',  ( -5.915653884842710930, 1.003805156977417345, 10.99560239355786351 ) ) ;
#1421 = LINE ( 'NONE', #10104, #7537 ) ;
#1422 = DIRECTION ( 'NONE',  ( 0.5877852522924802425, -0.8090169943749422332, 0.000000000000000000 ) ) ;
#1423 = VERTEX_POINT ( 'NONE', #10398 ) ;
#1424 = CARTESIAN_POINT ( 'NONE',  ( -6.403569081242510563E-16, 188.2499999989075263, 9.066987300000000971 ) ) ;
#1425 =( BOUNDED_CURVE ( )  B_SPLINE_CURVE ( 2, ( #5701, #11576, #12925, #9201, #13963, #3070, #14041, #7921, #15403 ),
 .UNSPECIFIED., .F., .F. ) 
 B_SPLINE_CURVE_WITH_KNOTS ( ( 3, 2, 2, 2, 3 ),
 ( 0.000000000000000000, 0.01785714285714285615, 0.03571428571428571230, 0.05357142857142856845, 0.07142857142857142461 ),
 .UNSPECIFIED. ) 
 CURVE ( )  GEOMETRIC_REPRESENTATION_ITEM ( )  RATIONAL_B_SPLINE_CURVE ( ( 1.000000000000000000, 0.9238795325112867385, 1.000000000000000000, 0.9238795325112867385, 1.000000000000000000, 0.9238795325112867385, 1.000000000000000000, 0.9238795325112867385, 1.000000000000000000 ) ) 
 REPRESENTATION_ITEM ( '' )  );
#1426 = VERTEX_POINT ( 'NONE', #8007 ) ;
#1427 = ADVANCED_FACE ( 'NONE', ( #12848 ), #1951, .F. ) ;
#1428 = ORIENTED_EDGE ( 'NONE', *, *, #582, .F. ) ;
#1429 = CARTESIAN_POINT ( 'NONE',  ( -3.420659742068546283, 4.931142898501624572, 25.49995053646222232 ) ) ;
#1430 = EDGE_LOOP ( 'NONE', ( #1210, #12509 ) ) ;
#1431 = CARTESIAN_POINT ( 'NONE',  ( 0.8561741729129451750, 2.066987299999999639, -1.399999998907525800 ) ) ;
#1432 = EDGE_CURVE ( 'NONE', #878, #13950, #13112, .T. ) ;
#1433 = FACE_BOUND ( 'NONE', #12661, .T. ) ;
#1434 = CARTESIAN_POINT ( 'NONE',  ( -1.815878914417024204, 228.0587508443335309, 9.590870893335578629 ) ) ;
#1435 = DIRECTION ( 'NONE',  ( -0.3090169943749584425, 0.9510565162951498674, 0.000000000000000000 ) ) ;
#1436 = CARTESIAN_POINT ( 'NONE',  ( -2.500000000000000444, 1.035533905932737753, 2.449999999999999734 ) ) ;
#1437 = DIRECTION ( 'NONE',  ( -0.000000000000000000, 1.000000000000000000, -0.000000000000000000 ) ) ;
#1438 = CARTESIAN_POINT ( 'NONE',  ( 4.005785023174503579, -4.467917056767357842, 31.79952054102714598 ) ) ;
#1439 = CARTESIAN_POINT ( 'NONE',  ( -2.066987299999999639, 0.8561741729129452860, 0.6000000010924748661 ) ) ;
#1440 = CARTESIAN_POINT ( 'NONE',  ( 0.000000000000000000, 0.4000000000000097367, 2.450963827680236129 ) ) ;
#1441 = CARTESIAN_POINT ( 'NONE',  ( -1.585166063744550602, 226.4701105292460568, 4.913902397277155387 ) ) ;
#1442 = EDGE_LOOP ( 'NONE', ( #5750, #13383 ) ) ;
#1443 = ORIENTED_EDGE ( 'NONE', *, *, #8639, .T. ) ;
#1444 = ORIENTED_EDGE ( 'NONE', *, *, #13970, .F. ) ;
#1445 = CARTESIAN_POINT ( 'NONE',  ( 5.317509234263979145, -2.779225709350955142, 30.86763921416088863 ) ) ;
#1446 = CARTESIAN_POINT ( 'NONE',  ( 1.742858872693429761, 189.0000000000000000, 5.171082332538968984 ) ) ;
#1447 = VERTEX_POINT ( 'NONE', #7771 ) ;
#1448 = CARTESIAN_POINT ( 'NONE',  ( 5.770331821586418108, -2.404225004693562262, 31.87380055247395561 ) ) ;
#1449 = CARTESIAN_POINT ( 'NONE',  ( 0.2623718222035119063, 6.245654667075785760, 4.026278297138354390 ) ) ;
#1450 = EDGE_CURVE ( 'NONE', #2495, #15690, #4190, .T. ) ;
#1451 = CARTESIAN_POINT ( 'NONE',  ( -3.107583187530470248, -5.133966411712660438, 18.87380682714710289 ) ) ;
#1452 = CARTESIAN_POINT ( 'NONE',  ( 4.435347140100928343, -4.403429997944614982, 24.49999999999999289 ) ) ;
#1453 = CARTESIAN_POINT ( 'NONE',  ( -6.844026213814746740E-16, 187.6999999978150697, 9.500000000000001776 ) ) ;
#1454 = CARTESIAN_POINT ( 'NONE',  ( 2.066987300000000527, 185.0499999989075093, 7.000000000000000000 ) ) ;
#1455 = CARTESIAN_POINT ( 'NONE',  ( -5.984759433607032442, 1.806271833852219899, 6.000082193215567905 ) ) ;
#1456 = CARTESIAN_POINT ( 'NONE',  ( -2.997451966578549065, 5.485105005465932493, 18.61517780375842790 ) ) ;
#1457 = PRODUCT_CONTEXT ( 'NONE', #7797, 'mechanical' ) ;
#1458 = EDGE_CURVE ( 'NONE', #6001, #1465, #12776, .T. ) ;
#1459 = CARTESIAN_POINT ( 'NONE',  ( 1.767766952966369320, 184.8699999975965511, 5.232233047033630235 ) ) ;
#1460 = CARTESIAN_POINT ( 'NONE',  ( -1.987493679921816137, 228.2178828950600860, 6.868649084925799286 ) ) ;
#1461 = CARTESIAN_POINT ( 'NONE',  ( -2.753288529192227774, 227.6732037325579654, 8.456785184543583966 ) ) ;
#1462 = AXIS2_PLACEMENT_3D ( 'NONE', #1507, #11295, #393 ) ;
#1463 = VECTOR ( 'NONE', #561, 1000.000000000000000 ) ;
#1464 = CARTESIAN_POINT ( 'NONE',  ( -2.880481771649630485, 189.8381383517797758, 8.187469944237161457 ) ) ;
#1465 = VERTEX_POINT ( 'NONE', #997 ) ;
#1466 = CARTESIAN_POINT ( 'NONE',  ( -5.935543223013850955, 0.8771126767607324570, 11.49999999999998224 ) ) ;
#1467 = LINE ( 'NONE', #8729, #1486 ) ;
#1468 = CARTESIAN_POINT ( 'NONE',  ( 2.897581130414634077E-17, -9.750000000000003553, 2.000000000000001776 ) ) ;
#1469 = CARTESIAN_POINT ( 'NONE',  ( 6.081590040723058976, 1.446205118473078199, 30.12632671364006143 ) ) ;
#1470 = CARTESIAN_POINT ( 'NONE',  ( 2.773164530494548696, 227.6577475117620679, 8.411308552413421680 ) ) ;
#1471 = AXIS2_PLACEMENT_3D ( 'NONE', #9482, #10912, #7021 ) ;
#1472 = EDGE_CURVE ( 'NONE', #10038, #12139, #7103, .T. ) ;
#1473 = DIRECTION ( 'NONE',  ( 0.000000000000000000, 0.000000000000000000, 1.000000000000000000 ) ) ;
#1474 = AXIS2_PLACEMENT_3D ( 'NONE', #10490, #14056, #15344 ) ;
#1475 = CARTESIAN_POINT ( 'NONE',  ( -2.066987299999999639, 0.8561741729129452860, -1.799999998907525267 ) ) ;
#1476 = CARTESIAN_POINT ( 'NONE',  ( -2.668367453516648169, -5.373994336898123336, 31.00000000000000000 ) ) ;
#1477 = FACE_OUTER_BOUND ( 'NONE', #11688, .T. ) ;
#1478 = CARTESIAN_POINT ( 'NONE',  ( -1.035533905932739529, 185.3499999999999659, 9.500000000000003553 ) ) ;
#1479 = CARTESIAN_POINT ( 'NONE',  ( -2.283493650000000041, 0.000000000000000000, 2.375000000546237278 ) ) ;
#1480 = CARTESIAN_POINT ( 'NONE',  ( 0.6402346998162695701, 228.8776282932165600, 8.774031424212344277 ) ) ;
#1481 = CARTESIAN_POINT ( 'NONE',  ( 0.8561741729129452860, 2.066987299999999639, -1.999999998907525445 ) ) ;
#1482 = CARTESIAN_POINT ( 'NONE',  ( -1.035533905932737753, 2.500000000000000444, -3.149999997815050801 ) ) ;
#1483 = CARTESIAN_POINT ( 'NONE',  ( -2.066987299999999639, 0.000000000000000000, 2.050000001092474822 ) ) ;
#1484 = CARTESIAN_POINT ( 'NONE',  ( 2.066987300000000083, 189.0999999989075206, 6.143825827087054492 ) ) ;
#1485 = CARTESIAN_POINT ( 'NONE',  ( 6.176542424588140179, -0.9554180641284089059, 17.99999999999998934 ) ) ;
#1486 = VECTOR ( 'NONE', #1702, 1000.000000000000000 ) ;
#1488 = ORIENTED_EDGE ( 'NONE', *, *, #10760, .F. ) ;
#1487 = CARTESIAN_POINT ( 'NONE',  ( -0.8561741729129455081, 186.2999999989075093, 4.933012699999999029 ) ) ;
#1489 = CARTESIAN_POINT ( 'NONE',  ( -4.267992336621228233, -4.217442018459970576, 17.73805675996853637 ) ) ;
#1490 = EDGE_CURVE ( 'NONE', #12426, #567, #3524, .T. ) ;
#1491 = CARTESIAN_POINT ( 'NONE',  ( -3.061616997868386099E-16, 189.0000000000000000, 7.000000000000000000 ) ) ;
#1492 = CARTESIAN_POINT ( 'NONE',  ( 6.172651332693098958, -0.9815532474593492429, 31.26190213084010949 ) ) ;
#1493 = CARTESIAN_POINT ( 'NONE',  ( -5.999999999999999112, 194.5935680195190116, 12.11154058223188379 ) ) ;
#1494 = CARTESIAN_POINT ( 'NONE',  ( -0.5042675786778498814, -6.230788509548846221, 12.37331068310445836 ) ) ;
#1495 = AXIS2_PLACEMENT_3D ( 'NONE', #5345, #8255, #14967 ) ;
#1496 = CARTESIAN_POINT ( 'NONE',  ( 3.106366801611882611, 5.134708448381354984, 17.12696220972948069 ) ) ;
#1497 = FACE_OUTER_BOUND ( 'NONE', #555, .T. ) ;
#1498 = AXIS2_PLACEMENT_3D ( 'NONE', #11832, #4612, #13110 ) ;
#1499 = CARTESIAN_POINT ( 'NONE',  ( -2.500000000000000444, 188.2499999978150527, 5.964466094067261359 ) ) ;
#1500 = CARTESIAN_POINT ( 'NONE',  ( 2.390857953333830554, 189.7853064097493530, 9.182117214708636510 ) ) ;
#1501 = CARTESIAN_POINT ( 'NONE',  ( -2.841519077896177858, 5.566940434250000180, 30.73620383159193281 ) ) ;
#1502 = CARTESIAN_POINT ( 'NONE',  ( -5.842945980534642203, -1.369128644668982542, 12.37378430870260537 ) ) ;
#1503 = CARTESIAN_POINT ( 'NONE',  ( -5.866923913994629203, -1.260079467906603634, 10.70047945897284158 ) ) ;
#1504 = EDGE_LOOP ( 'NONE', ( #9820, #5203, #3418, #12305 ) ) ;
#1505 = CARTESIAN_POINT ( 'NONE',  ( 2.066987300000000083, 186.0499999989075093, 7.000000000000000000 ) ) ;
#1506 = ORIENTED_EDGE ( 'NONE', *, *, #1759, .T. ) ;
#1507 = CARTESIAN_POINT ( 'NONE',  ( 0.000000000000000000, 0.000000000000000000, 5.000000000000004441 ) ) ;
#1508 =( GEOMETRIC_REPRESENTATION_CONTEXT ( 3 ) GLOBAL_UNCERTAINTY_ASSIGNED_CONTEXT ( ( #10618 ) ) GLOBAL_UNIT_ASSIGNED_CONTEXT ( ( #14072, #5503, #3106 ) ) REPRESENTATION_CONTEXT ( 'NONE', 'WORKASPACE' ) );
#1509 = ORIENTED_EDGE ( 'NONE', *, *, #68, .T. ) ;
#1510 = CARTESIAN_POINT ( 'NONE',  ( -5.866984344570797205, -1.259800266528794843, 25.29931806258175087 ) ) ;
#1511 = FACE_OUTER_BOUND ( 'NONE', #12331, .T. ) ;
#1512 = VERTEX_POINT ( 'NONE', #1232 ) ;
#1513 = CARTESIAN_POINT ( 'NONE',  ( -0.8561741729129458411, -2.066987299999999195, -0.9999999989075254447 ) ) ;
#1514 = CARTESIAN_POINT ( 'NONE',  ( 0.9737778612005509871, 5.920671847850518255, 4.737363758846515616 ) ) ;
#1515 = CARTESIAN_POINT ( 'NONE',  ( -1.055448890735882106, 228.1934063406578446, 9.986798501930948646 ) ) ;
#1516 = FACE_OUTER_BOUND ( 'NONE', #4435, .T. ) ;
#1517 = CARTESIAN_POINT ( 'NONE',  ( -2.500000000000000000, 0.000000000000000000, 0.09999999999999982514 ) ) ;
#1518 = CARTESIAN_POINT ( 'NONE',  ( -2.668367453516831134, 5.373994336898032742, 17.99999999999998934 ) ) ;
#1519 = ADVANCED_FACE ( 'NONE', ( #3542, #41 ), #8413, .T. ) ;
#1520 = MECHANICAL_DESIGN_GEOMETRIC_PRESENTATION_REPRESENTATION (  '', ( #15246 ), #9915 ) ;
#1521 = PLANE ( 'NONE',  #8777 ) ;
#1522 = CARTESIAN_POINT ( 'NONE',  ( 2.066987299999999639, 2.531329380823229670E-16, -0.5499999989075250451 ) ) ;
#1523 = CARTESIAN_POINT ( 'NONE',  ( 5.558508435838260375, -2.857531096718793240, 11.49999999999998224 ) ) ;
#1524 = CARTESIAN_POINT ( 'NONE',  ( -1.035533905932737975, 186.5499999978150356, 4.500000000000001776 ) ) ;
#1525 = EDGE_CURVE ( 'NONE', #13850, #13656, #6944, .T. ) ;
#1526 = ORIENTED_EDGE ( 'NONE', *, *, #2897, .T. ) ;
#1527 = EDGE_LOOP ( 'NONE', ( #2291, #5119 ) ) ;
#1528 = EDGE_CURVE ( 'NONE', #13930, #12389, #6542, .T. ) ;
#1529 = ORIENTED_EDGE ( 'NONE', *, *, #11347, .T. ) ;
#1530 = CARTESIAN_POINT ( 'NONE',  ( 0.7995298244855962855, 5.947211616899230613, 18.61456014619857413 ) ) ;
#1531 = CARTESIAN_POINT ( 'NONE',  ( 2.392413149609226686, 188.9999999999999716, 7.742749228504306025 ) ) ;
#1532 = VERTEX_POINT ( 'NONE', #14606 ) ;
#1533 = CARTESIAN_POINT ( 'NONE',  ( -5.984759433606969381, -1.806271833852430397, 16.99991780678442410 ) ) ;
#1534 = CARTESIAN_POINT ( 'NONE',  ( -4.142620314836390705, -4.341347824677495026, 18.61442521571937192 ) ) ;
#1535 = EDGE_CURVE ( 'NONE', #2787, #6307, #4658, .T. ) ;
#1536 = CYLINDRICAL_SURFACE ( 'NONE', #14676, 2.000000000000000000 ) ;
#1537 = CARTESIAN_POINT ( 'NONE',  ( 0.9999171162591148354, 6.169494774098524204, 17.86722320330678215 ) ) ;
#1538 = CARTESIAN_POINT ( 'NONE',  ( -1.767766952966369765, 186.7999999978150356, 8.767766952966368876 ) ) ;
#1539 = PRESENTATION_STYLE_ASSIGNMENT (( #6491 ) ) ;
#1540 = DIRECTION ( 'NONE',  ( 0.000000000000000000, 1.000000000000000000, 0.000000000000000000 ) ) ;
#1541 = CARTESIAN_POINT ( 'NONE',  ( -4.416837305303601191, 4.422286678978908370, 18.26190213084011660 ) ) ;
#1542 = DIRECTION ( 'NONE',  ( 0.000000000000000000, 1.000000000000000000, 0.000000000000000000 ) ) ;
#1543 = CARTESIAN_POINT ( 'NONE',  ( -2.500000000000000444, 185.2199999975965738, 8.035533905932737753 ) ) ;
#1544 = CARTESIAN_POINT ( 'NONE',  ( 0.8818167416564541838, 227.6759890937897239, 5.303628879260831042 ) ) ;
#1545 = CARTESIAN_POINT ( 'NONE',  ( -1.104351905119298705, 226.3927175376774699, 4.685770134608635118 ) ) ;
#1546 = CARTESIAN_POINT ( 'NONE',  ( -1.934526094385236483, 189.7531569016572632, 9.674728188581434907 ) ) ;
#1547 = B_SPLINE_CURVE_WITH_KNOTS ( 'NONE', 3,
 ( #15097, #11740, #843, #5708, #10551 ),
 .UNSPECIFIED., .F., .F.,
 ( 4, 1, 4 ),
 ( 0.7688659053744423266, 0.7708896602024635225, 0.7729134150304846074 ),
 .UNSPECIFIED. ) ;
#1548 = EDGE_LOOP ( 'NONE', ( #959, #8690, #8357, #5866 ) ) ;
#1549 = CARTESIAN_POINT ( 'NONE',  ( -6.021167129161051790, 1.680051667990315023, 17.02640428276697904 ) ) ;
#1550 = CARTESIAN_POINT ( 'NONE',  ( -6.105925084677665815, 1.337450587213249165, 23.70066851092423477 ) ) ;
#1551 = DIRECTION ( 'NONE',  ( 0.000000000000000000, 0.000000000000000000, 1.000000000000000000 ) ) ;
#1552 = CARTESIAN_POINT ( 'NONE',  ( 6.155912734541118425, 1.081577393120980224, 30.49610786875027912 ) ) ;
#1553 = CARTESIAN_POINT ( 'NONE',  ( 2.968835193067500988, 227.4419886495170715, 7.776466547877070923 ) ) ;
#1554 = CARTESIAN_POINT ( 'NONE',  ( -3.255013540813579187, -5.336859797930871174, 31.87381964045071214 ) ) ;
#1555 = ADVANCED_FACE ( 'NONE', ( #6762 ), #12860, .F. ) ;
#1556 = CARTESIAN_POINT ( 'NONE',  ( 1.035533905932739085, -2.500000000000000000, 1.150000000000000133 ) ) ;
#1557 = CARTESIAN_POINT ( 'NONE',  ( 5.317509234263970264, -2.779225709350972906, 5.000000000000004441 ) ) ;
#1558 =( NAMED_UNIT ( * ) SI_UNIT ( $, .STERADIAN. ) SOLID_ANGLE_UNIT ( ) );
#1559 = CARTESIAN_POINT ( 'NONE',  ( -2.817313151351126699, -5.579000502529464001, 30.86762589283693359 ) ) ;
#1560 = CARTESIAN_POINT ( 'NONE',  ( -1.767766952966369098, 185.0999999999999943, 5.232233047033630235 ) ) ;
#1561 = CARTESIAN_POINT ( 'NONE',  ( 2.000000000000001776, 0.000000000000000000, 0.000000000000000000 ) ) ;
#1562 = CARTESIAN_POINT ( 'NONE',  ( -1.454198809819935878, 227.8150368499753995, 5.705206729889046535 ) ) ;
#1563 = CARTESIAN_POINT ( 'NONE',  ( 0.000000000000000000, 0.000000000000000000, -2.500000000000000000 ) ) ;
#1564 = EDGE_CURVE ( 'NONE', #1161, #1036, #8266, .T. ) ;
#1565 = CARTESIAN_POINT ( 'NONE',  ( -1.767766952966368432, -1.767766952966369320, -2.899999997815050357 ) ) ;
#1566 = CARTESIAN_POINT ( 'NONE',  ( 2.066987300000000083, -0.8561741729129450640, 1.092474635061568626E-09 ) ) ;
#1567 = CARTESIAN_POINT ( 'NONE',  ( 2.066987300000000083, 188.2999999989075093, 6.143825827087054492 ) ) ;
#1568 = CARTESIAN_POINT ( 'NONE',  ( -5.317509234263866347, -2.779225709351170970, 18.13064961348854709 ) ) ;
#1570 = VERTEX_POINT ( 'NONE', #10257 ) ;
#1569 = CARTESIAN_POINT ( 'NONE',  ( -1.461580736456473462, 188.1499999989075320, 8.461580736456472351 ) ) ;
#1571 = CARTESIAN_POINT ( 'NONE',  ( -3.107688324358743426, -5.133887830459814339, 17.12621569129736798 ) ) ;
#1572 = CARTESIAN_POINT ( 'NONE',  ( 1.767766952966368432, 186.9999999978150527, 8.767766952966368876 ) ) ;
#1573 = CARTESIAN_POINT ( 'NONE',  ( 3.659182332138577465E-16, 221.4150671951173308, 6.196499129422101682 ) ) ;
#1574 = CARTESIAN_POINT ( 'NONE',  ( 4.322356511625632614, 7.650514973136570696, 31.00000000000000000 ) ) ;
#1575 = CARTESIAN_POINT ( 'NONE',  ( -2.500000000000000000, 0.000000000000000000, 0.09999999999999982514 ) ) ;
#1576 = CARTESIAN_POINT ( 'NONE',  ( 1.447897648385842562, 188.9999999996366569, 4.953942678156875168 ) ) ;
#1577 = DIRECTION ( 'NONE',  ( -1.062480551894329776E-17, -2.775557561562888393E-16, 1.000000000000000000 ) ) ;
#1578 = CARTESIAN_POINT ( 'NONE',  ( 1.410416696976425799, 190.0533888663666175, 4.554553427631445217 ) ) ;
#1579 = CARTESIAN_POINT ( 'NONE',  ( 4.322356511625649489, 7.650514973136559149, 5.000000000000004441 ) ) ;
#1580 = CARTESIAN_POINT ( 'NONE',  ( -5.329907877631328006, -2.755840666746313339, 11.76194324003145475 ) ) ;
#1581 = FACE_OUTER_BOUND ( 'NONE', #15550, .T. ) ;
#1582 = ORIENTED_EDGE ( 'NONE', *, *, #1139, .F. ) ;
#1583 = CARTESIAN_POINT ( 'NONE',  ( 2.066987300000000083, 186.8499999989075206, 7.000000000000000000 ) ) ;
#1584 = VERTEX_POINT ( 'NONE', #4207 ) ;
#1585 = CARTESIAN_POINT ( 'NONE',  ( -5.931734679891415674, -0.9039278060246241919, 24.23617396794404044 ) ) ;
#1586 = ORIENTED_EDGE ( 'NONE', *, *, #13291, .F. ) ;
#1587 = AXIS2_PLACEMENT_3D ( 'NONE', #5525, #1773, #9037 ) ;
#1588 = CARTESIAN_POINT ( 'NONE',  ( -5.903119516422441038, -1.077859910107684227, 25.11519382448850379 ) ) ;
#1589 = FILL_AREA_STYLE_COLOUR ( '', #14448 ) ;
#1590 = ORIENTED_EDGE ( 'NONE', *, *, #15629, .T. ) ;
#1591 = CARTESIAN_POINT ( 'NONE',  ( 0.8561741729129451750, 2.066987299999999639, -2.199999998907525622 ) ) ;
#1592 = CARTESIAN_POINT ( 'NONE',  ( -1.000049560716421482, 5.916071405810168216, 17.86967799011532776 ) ) ;
#1593 = CARTESIAN_POINT ( 'NONE',  ( -2.986011043896227513, 189.8622845448325052, 7.656297732253541710 ) ) ;
#1594 = CARTESIAN_POINT ( 'NONE',  ( 6.123233995736766282E-16, -6.250000000000000888, 6.000000000000005329 ) ) ;
#1595 = CARTESIAN_POINT ( 'NONE',  ( 0.9662756667218489470, 2.500000000000000000, -2.546655916391819652 ) ) ;
#1596 = CARTESIAN_POINT ( 'NONE',  ( -4.143041610105331785, -4.340967609747012013, 10.88602261056916021 ) ) ;
#1597 = CARTESIAN_POINT ( 'NONE',  ( -6.021167129161005604, -1.680051667990481779, 25.47359571723300320 ) ) ;
#1598 = CARTESIAN_POINT ( 'NONE',  ( -1.461580736456472795, 1.461580736456472795, 0.5500000010924748217 ) ) ;
#1599 = VECTOR ( 'NONE', #719, 1000.000000000000114 ) ;
#1600 = CARTESIAN_POINT ( 'NONE',  ( -5.726307184802663208, 2.506131700382440819, 30.19973484982324763 ) ) ;
#1601 = DIRECTION ( 'NONE',  ( 0.000000000000000000, 0.000000000000000000, 1.000000000000000000 ) ) ;
#1602 = ORIENTED_EDGE ( 'NONE', *, *, #12992, .T. ) ;
#1603 = ORIENTED_EDGE ( 'NONE', *, *, #7772, .F. ) ;
#1604 = ORIENTED_EDGE ( 'NONE', *, *, #4264, .T. ) ;
#1605 = LINE ( 'NONE', #2653, #14618 ) ;
#1606 = CARTESIAN_POINT ( 'NONE',  ( 0.2265647687538700217, 188.9999999999999716, 9.493607779905927302 ) ) ;
#1607 = ORIENTED_EDGE ( 'NONE', *, *, #15050, .F. ) ;
#1608 = CARTESIAN_POINT ( 'NONE',  ( -2.897581130414634077E-17, 19.99999999999999645, -8.250000000000003553 ) ) ;
#1609 = CONICAL_SURFACE ( 'NONE', #3645, 4.000000000000002665, 0.1745329251994333364 ) ;
#1610 = EDGE_CURVE ( 'NONE', #4214, #15156, #15345, .T. ) ;
#1611 = CARTESIAN_POINT ( 'NONE',  ( -2.668367453516752530, -5.373994336898073598, 18.13236078583909361 ) ) ;
#1612 = CARTESIAN_POINT ( 'NONE',  ( -3.158825713737541729, 5.393784879207139227, 31.79933148907577234 ) ) ;
#1613 = CARTESIAN_POINT ( 'NONE',  ( 2.817313151350985034, 5.579000502529534167, 17.99999999999998934 ) ) ;
#1614 = CARTESIAN_POINT ( 'NONE',  ( -2.500000000000000444, 186.6999999978150697, 7.000000000000000000 ) ) ;
#1615 = DIRECTION ( 'NONE',  ( -0.000000000000000000, 1.000000000000000000, -0.000000000000000000 ) ) ;
#1616 = CARTESIAN_POINT ( 'NONE',  ( 2.500000000000000444, 1.035533905932737975, 1.356999999978150573 ) ) ;
#1617 = CARTESIAN_POINT ( 'NONE',  ( 5.935543223013866942, 0.8771126767606117758, 17.99999999999998934 ) ) ;
#1618 = DIRECTION ( 'NONE',  ( 1.000000000000000000, 0.000000000000000000, 0.000000000000000000 ) ) ;
#1619 = CARTESIAN_POINT ( 'NONE',  ( -2.500000000000000444, 186.0199999975965568, 8.035533905932737753 ) ) ;
#1620 = CARTESIAN_POINT ( 'NONE',  ( -1.212431555520800508, 228.7775460029053534, 8.484988061474600940 ) ) ;
#1621 = CARTESIAN_POINT ( 'NONE',  ( -2.191511056945971259, 226.6300844452854903, 5.385369267317587472 ) ) ;
#1622 = ADVANCED_FACE ( 'NONE', ( #14135 ), #15187, .T. ) ;
#1623 = CARTESIAN_POINT ( 'NONE',  ( -2.353560662074906773, 189.1623160119228544, 9.042440134401656948 ) ) ;
#1624 = ORIENTED_EDGE ( 'NONE', *, *, #4651, .T. ) ;
#1625 = CARTESIAN_POINT ( 'NONE',  ( -2.692215568229806788, 5.362327947133613826, 5.262290378359323562 ) ) ;
#1626 = AXIS2_PLACEMENT_3D ( 'NONE', #3473, #1885, #6759 ) ;
#1627 = EDGE_CURVE ( 'NONE', #1738, #3723, #666, .T. ) ;
#1628 = CARTESIAN_POINT ( 'NONE',  ( -5.558508435838219519, 2.857531096718872732, 31.00000000000000000 ) ) ;
#1629 = CARTESIAN_POINT ( 'NONE',  ( -3.312341048453600667, 5.004306261885368201, 23.52601979877760385 ) ) ;
#1630 = CARTESIAN_POINT ( 'NONE',  ( 0.1323602877614195317, 5.999999999999997335, 25.50000000000000355 ) ) ;
#1631 = CARTESIAN_POINT ( 'NONE',  ( 2.988911113477941583, 227.2040587690521534, 7.075956526733278018 ) ) ;
#1632 = CARTESIAN_POINT ( 'NONE',  ( 4.153663429050769906, 4.670992970568382141, 5.799331489075774115 ) ) ;
#1633 = CARTESIAN_POINT ( 'NONE',  ( 1.767766952966369320, -1.767766952966368654, 2.000000000000000000 ) ) ;
#1634 = CARTESIAN_POINT ( 'NONE',  ( -2.500000000000001776, 188.4500000000000171, 8.035533905932737753 ) ) ;
#1635 = CARTESIAN_POINT ( 'NONE',  ( 2.500000000000000444, 185.5500000000000114, 8.035533905932739529 ) ) ;
#1636 = CARTESIAN_POINT ( 'NONE',  ( -1.035533905932738197, -2.500000000000000000, -0.5500000000000001554 ) ) ;
#1637 = AXIS2_PLACEMENT_3D ( 'NONE', #11385, #486, #15285 ) ;
#1638 = CARTESIAN_POINT ( 'NONE',  ( 0.8818167416564541838, 227.6759890937897239, 5.303628879260831042 ) ) ;
#1639 = CARTESIAN_POINT ( 'NONE',  ( 2.066987299999999639, 0.8561741729129456191, -2.099999998907525534 ) ) ;
#1640 = EDGE_CURVE ( 'NONE', #8395, #9339, #1014, .T. ) ;
#1641 = CARTESIAN_POINT ( 'NONE',  ( -4.416837305303488392, -4.422286678979018504, 11.23809786915986564 ) ) ;
#1642 = CARTESIAN_POINT ( 'NONE',  ( 0.8561741729129452860, 2.066987299999999639, 1.000000001092474555 ) ) ;
#1643 = CARTESIAN_POINT ( 'NONE',  ( -2.066987300000001415, 187.7999999989075093, 6.143825827087054492 ) ) ;
#1644 = CARTESIAN_POINT ( 'NONE',  ( 5.616089948629791273, -2.743103014345418700, 18.50436969680152899 ) ) ;
#1646 = ORIENTED_EDGE ( 'NONE', *, *, #2416, .F. ) ;
#1645 = CARTESIAN_POINT ( 'NONE',  ( 2.066987299999999195, 188.3999999989075320, 7.856174172912946396 ) ) ;
#1647 = PLANE ( 'NONE',  #4070 ) ;
#1648 = CYLINDRICAL_SURFACE ( 'NONE', #15697, 1.000000000000000444 ) ;
#1649 = ADVANCED_FACE ( 'NONE', ( #12149 ), #14287, .T. ) ;
#1650 = CARTESIAN_POINT ( 'NONE',  ( 0.8499999999999896527, 0.4000000000000097367, -2.619018321873355593 ) ) ;
#1651 = DIRECTION ( 'NONE',  ( 1.000000000000000000, 0.000000000000000000, 0.000000000000000000 ) ) ;
#1652 = CARTESIAN_POINT ( 'NONE',  ( 1.292454554785913867, 188.9999999995436610, 9.144800990124029028 ) ) ;
#1653 = CARTESIAN_POINT ( 'NONE',  ( -2.500000000000000888, 188.2999999978150356, 7.000000000000000000 ) ) ;
#1654 = EDGE_CURVE ( 'NONE', #2649, #5182, #11988, .T. ) ;
#1655 = CARTESIAN_POINT ( 'NONE',  ( 4.286401442266591921, -4.198423832313132209, 5.000000000000004441 ) ) ;
#1656 = CARTESIAN_POINT ( 'NONE',  ( 5.558508435838322548, -2.857531096718671115, 24.49999999999999289 ) ) ;
#1657 = CARTESIAN_POINT ( 'NONE',  ( 0.7081379353438682633, -0.3999999999999898637, 2.606463079733445376 ) ) ;
#1658 = DIRECTION ( 'NONE',  ( -0.000000000000000000, 1.000000000000000000, -0.000000000000000000 ) ) ;
#1659 = ORIENTED_EDGE ( 'NONE', *, *, #3570, .F. ) ;
#1660 = CARTESIAN_POINT ( 'NONE',  ( -1.084202172485504434E-16, 187.8499999989074922, 4.933012699999999029 ) ) ;
#1661 = AXIS2_PLACEMENT_3D ( 'NONE', #4362, #10562, #11676 ) ;
#1662 = ORIENTED_EDGE ( 'NONE', *, *, #10649, .T. ) ;
#1663 = CARTESIAN_POINT ( 'NONE',  ( -5.317509234263939177, 2.779225709351033302, 11.49999999999998224 ) ) ;
#1664 = EDGE_LOOP ( 'NONE', ( #12566, #10687, #3663, #8050 ) ) ;
#1665 = LINE ( 'NONE', #12794, #2767 ) ;
#1666 = DIRECTION ( 'NONE',  ( 0.5877852522924802425, -0.8090169943749422332, 0.000000000000000000 ) ) ;
#1667 = EDGE_LOOP ( 'NONE', ( #3249, #5046 ) ) ;
#1668 = CARTESIAN_POINT ( 'NONE',  ( -1.265664690411614835E-16, 2.066987299999999639, 0.2500000010924746663 ) ) ;
#1669 = CARTESIAN_POINT ( 'NONE',  ( 0.9739805876848001143, 5.920636045238165224, 5.261713868144209272 ) ) ;
#1670 = EDGE_CURVE ( 'NONE', #9215, #1760, #9453, .T. ) ;
#1671 = CARTESIAN_POINT ( 'NONE',  ( 1.461580736456472351, 189.1499999989075320, 8.461580736456474128 ) ) ;
#1672 = CARTESIAN_POINT ( 'NONE',  ( 2.500000000000000000, 3.061616997868383141E-16, -1.100000000000000311 ) ) ;
#1673 = CARTESIAN_POINT ( 'NONE',  ( -5.859221468178966497, -2.178708437343180204, 5.974085423341712442 ) ) ;
#1674 = CARTESIAN_POINT ( 'NONE',  ( -2.692215568229781031, -5.362327947133626260, 11.23770962164069687 ) ) ;
#1675 = CARTESIAN_POINT ( 'NONE',  ( -5.648559266344434171, -2.676764518776131307, 25.11396179408071205 ) ) ;
#1676 = CARTESIAN_POINT ( 'NONE',  ( -0.8561741729129455081, 2.066987299999999639, -1.099999998907525089 ) ) ;
#1677 = CARTESIAN_POINT ( 'NONE',  ( -0.5039005892421096755, 6.230833003620542598, 30.12636388911297658 ) ) ;
#1678 = VERTEX_POINT ( 'NONE', #14213 ) ;
#1679 = EDGE_LOOP ( 'NONE', ( #2885, #13212 ) ) ;
#1680 = CIRCLE ( 'NONE', #12608, 1.499999999999999556 ) ;
#1681 = VERTEX_POINT ( 'NONE', #3394 ) ;
#1682 = CARTESIAN_POINT ( 'NONE',  ( 0.000000000000000000, 6.250000000000000888, 12.49999999999998401 ) ) ;
#1683 = CARTESIAN_POINT ( 'NONE',  ( 7.180990026460741582, -3.384707322287397790, 5.000000000000004441 ) ) ;
#1684 = ORIENTED_EDGE ( 'NONE', *, *, #2925, .F. ) ;
#1685 = CARTESIAN_POINT ( 'NONE',  ( 0.2637975869347833902, 6.245592211692893692, 5.973328399491914631 ) ) ;
#1686 = CARTESIAN_POINT ( 'NONE',  ( 0.2622916576876764272, -5.995491482261826377, 31.97384942646813855 ) ) ;
#1687 = CARTESIAN_POINT ( 'NONE',  ( -5.486741141153813395, 2.429871531109682792, 5.798882422479413101 ) ) ;
#1688 = CARTESIAN_POINT ( 'NONE',  ( 0.9740012993921304263, 6.173846968979621153, 18.26164920628446708 ) ) ;
#1689 = CARTESIAN_POINT ( 'NONE',  ( 1.035533905932738419, 185.3499999978151038, 9.500000000000003553 ) ) ;
#1690 = FACE_OUTER_BOUND ( 'NONE', #9959, .T. ) ;
#1691 = AXIS2_PLACEMENT_3D ( 'NONE', #6918, #13984, #7870 ) ;
#1692 = CARTESIAN_POINT ( 'NONE',  ( -4.435347140101169927, 4.403429997944371621, 18.13063932754211294 ) ) ;
#1693 = CARTESIAN_POINT ( 'NONE',  ( 0.000000000000000000, 0.000000000000000000, 0.000000000000000000 ) ) ;
#1694 = CARTESIAN_POINT ( 'NONE',  ( -1.767766952966369098, 185.8699999975965511, 5.232233047033630235 ) ) ;
#1695 = CARTESIAN_POINT ( 'NONE',  ( 1.057043591443594943, 228.1937260751906820, 9.987734910156856216 ) ) ;
#1696 = CARTESIAN_POINT ( 'NONE',  ( -1.585166063744550602, 226.4701105292460568, 4.913902397277155387 ) ) ;
#1697 = ADVANCED_FACE ( 'NONE', ( #5876 ), #14538, .F. ) ;
#1698 = EDGE_LOOP ( 'NONE', ( #15231, #87, #3481, #13122 ) ) ;
#1699 = CARTESIAN_POINT ( 'NONE',  ( 2.460891429721819179, -0.4634845133093605241, -2.499202848233824881 ) ) ;
#1700 = ORIENTED_EDGE ( 'NONE', *, *, #6004, .T. ) ;
#1701 = CARTESIAN_POINT ( 'NONE',  ( 3.118365096457674568, 189.0000000000000000, -7.000000000000000888 ) ) ;
#1702 = DIRECTION ( 'NONE',  ( -0.000000000000000000, -1.000000000000000000, -0.000000000000000000 ) ) ;
#1703 = CARTESIAN_POINT ( 'NONE',  ( 0.8738043859791279067, -6.188821459035870554, 12.00341560223749759 ) ) ;
#1704 = CARTESIAN_POINT ( 'NONE',  ( 5.558508435838199979, 2.857531096718914476, 30.86762589283693359 ) ) ;
#1705 = FACE_OUTER_BOUND ( 'NONE', #4012, .T. ) ;
#1706 = CARTESIAN_POINT ( 'NONE',  ( -4.154121946520862529, -4.670585111242981036, 31.79887838423339019 ) ) ;
#1707 = CARTESIAN_POINT ( 'NONE',  ( 1.767766952966368654, 1.767766952966369098, 1.399999999999999911 ) ) ;
#1708 = CARTESIAN_POINT ( 'NONE',  ( -4.286401442266545736, -4.198423832313181059, 31.13061695532138984 ) ) ;
#1709 = EDGE_CURVE ( 'NONE', #202, #338, #11413, .T. ) ;
#1710 = CARTESIAN_POINT ( 'NONE',  ( 5.783198643800754546, 1.602922020054761365, 5.973778239432934178 ) ) ;
#1711 = CARTESIAN_POINT ( 'NONE',  ( -2.500000000000000888, 187.5999999999999943, 7.000000000000000000 ) ) ;
#1712 = AXIS2_PLACEMENT_3D ( 'NONE', #13073, #8239, #10852 ) ;
#1713 = EDGE_CURVE ( 'NONE', #10824, #5765, #15504, .T. ) ;
#1714 = CARTESIAN_POINT ( 'NONE',  ( -0.7328022267957914337, 227.6546247107034446, 5.241927322362504249 ) ) ;
#1715 = CARTESIAN_POINT ( 'NONE',  ( -9.750000000000003553, 184.0000000000000000, -3.401296724241641415E-14 ) ) ;
#1716 = CARTESIAN_POINT ( 'NONE',  ( 2.930922878467443038, 5.520395124723591174, 12.00389213124966759 ) ) ;
#1717 = EDGE_CURVE ( 'NONE', #15426, #9324, #13100, .T. ) ;
#1718 = CARTESIAN_POINT ( 'NONE',  ( 3.796994071234844259E-16, -2.066987299999999639, -0.9499999989075252893 ) ) ;
#1719 = CARTESIAN_POINT ( 'NONE',  ( -2.066987300000000971, 187.8499999989074922, 7.000000000000000000 ) ) ;
#1720 = CARTESIAN_POINT ( 'NONE',  ( -4.143041610105435701, 4.340967609746908096, 18.61397738943082203 ) ) ;
#1721 = AXIS2_PLACEMENT_3D ( 'NONE', #13992, #15511, #9156 ) ;
#1723 = ORIENTED_EDGE ( 'NONE', *, *, #12237, .T. ) ;
#1722 = CARTESIAN_POINT ( 'NONE',  ( -2.066987300000000083, 187.1999999989075434, 6.143825827087054492 ) ) ;
#1724 = CARTESIAN_POINT ( 'NONE',  ( -4.196038884587234286, -4.289036423669209341, 17.49610204984018580 ) ) ;
#1725 = VECTOR ( 'NONE', #7804, 1000.000000000000000 ) ;
#1726 = DIRECTION ( 'NONE',  ( -6.123233995736766036E-17, 1.000000000000000000, 0.000000000000000000 ) ) ;
#1727 = CARTESIAN_POINT ( 'NONE',  ( 0.000000000000000000, 185.8606548077538321, 9.048340948986950849 ) ) ;
#1728 = SURFACE_STYLE_FILL_AREA ( #15106 ) ;
#1729 = CARTESIAN_POINT ( 'NONE',  ( 1.382634503510036250, 189.0823306087117430, 9.850504157829032437 ) ) ;
#1730 = CYLINDRICAL_SURFACE ( 'NONE', #6064, 1.000000000000000666 ) ;
#1731 = CARTESIAN_POINT ( 'NONE',  ( -1.000049560716534502, 5.916071405810148676, 30.86967799011533486 ) ) ;
#1732 = CARTESIAN_POINT ( 'NONE',  ( 2.866460994376960336, 189.9235028716541933, 6.357051353814127559 ) ) ;
#1734 = CARTESIAN_POINT ( 'NONE',  ( 5.725930890718318622, -2.506952462184073749, 5.799331489075775004 ) ) ;
#1733 = VECTOR ( 'NONE', #8292, 1000.000000000000000 ) ;
#1735 = LINE ( 'NONE', #11443, #8822 ) ;
#1736 = AXIS2_PLACEMENT_3D ( 'NONE', #2792, #8928, #476 ) ;
#1737 = CARTESIAN_POINT ( 'NONE',  ( -5.486741141153752999, -2.429871531109820904, 10.70111757752057358 ) ) ;
#1738 = VERTEX_POINT ( 'NONE', #10723 ) ;
#1739 = CARTESIAN_POINT ( 'NONE',  ( -0.8561741729129455081, 186.2999999989075093, 4.933012699999999029 ) ) ;
#1740 = ORIENTED_EDGE ( 'NONE', *, *, #8830, .T. ) ;
#1741 = CARTESIAN_POINT ( 'NONE',  ( 7.490007020835728113, -2.433650805992114918, 17.99999999999998934 ) ) ;
#1742 = ORIENTED_EDGE ( 'NONE', *, *, #9903, .T. ) ;
#1743 = CYLINDRICAL_SURFACE ( 'NONE', #1746, 2.499999999999999556 ) ;
#1744 = CYLINDRICAL_SURFACE ( 'NONE', #10390, 1.000000000000000666 ) ;
#1745 = ORIENTED_EDGE ( 'NONE', *, *, #3115, .T. ) ;
#1746 = AXIS2_PLACEMENT_3D ( 'NONE', #5265, #10342, #12567 ) ;
#1747 = CARTESIAN_POINT ( 'NONE',  ( 0.8561741729129463963, -2.066987299999999195, -2.499999998907525445 ) ) ;
#1748 = CARTESIAN_POINT ( 'NONE',  ( -5.935543223013847403, -0.8771126767607489993, 5.000000000000004441 ) ) ;
#1749 = CARTESIAN_POINT ( 'NONE',  ( 2.031800923730693940E-13, -6.250000000000000888, 23.49999999999999289 ) ) ;
#1750 = EDGE_CURVE ( 'NONE', #2410, #3136, #2201, .T. ) ;
#1751 = CARTESIAN_POINT ( 'NONE',  ( 1.767766952966368654, 1.767766952966369098, 1.500000002184949777 ) ) ;
#1752 = CARTESIAN_POINT ( 'NONE',  ( -1.035533905932737753, 2.500000000000000444, 2.350000000000000533 ) ) ;
#1753 = CARTESIAN_POINT ( 'NONE',  ( -3.923477796648659144, 4.541042560386356897, 17.12696220972948069 ) ) ;
#1754 = ITEM_DEFINED_TRANSFORMATION ( 'NONE', 'NONE', #11121,  #14201 ) ;
#1755 = CARTESIAN_POINT ( 'NONE',  ( 7.490007020835692586, -2.433650805992223720, 31.00000000000000000 ) ) ;
#1756 = CARTESIAN_POINT ( 'NONE',  ( -2.066987299999999639, 0.8561741729129452860, -1.799999998907525267 ) ) ;
#1757 = CARTESIAN_POINT ( 'NONE',  ( -1.000049271338467216, 6.169473353325554577, 30.86969612704551835 ) ) ;
#1758 = ORIENTED_EDGE ( 'NONE', *, *, #2692, .T. ) ;
#1759 = EDGE_CURVE ( 'NONE', #5575, #5516, #1039, .T. ) ;
#1760 = VERTEX_POINT ( 'NONE', #3321 ) ;
#1761 = ORIENTED_EDGE ( 'NONE', *, *, #8988, .T. ) ;
#1762 = CARTESIAN_POINT ( 'NONE',  ( 4.435347140101026042, -4.403429997944519059, 11.63234125634166105 ) ) ;
#1763 = DIRECTION ( 'NONE',  ( 0.000000000000000000, 1.000000000000000000, 0.000000000000000000 ) ) ;
#1764 = ORIENTED_EDGE ( 'NONE', *, *, #3943, .F. ) ;
#1765 = CARTESIAN_POINT ( 'NONE',  ( 5.329945432499675562, -2.755769831645047852, 18.26229037835932090 ) ) ;
#1766 = CARTESIAN_POINT ( 'NONE',  ( -1.767766952966369098, 1.767766952966369098, 0.1000000021849495324 ) ) ;
#1767 = CARTESIAN_POINT ( 'NONE',  ( -0.8736772044958448502, 6.188841968496081591, 17.49611573292807520 ) ) ;
#1768 = COLOUR_RGB ( '', 0.31764706, 0.68627451, 0.89019608) ;
#1769 = CARTESIAN_POINT ( 'NONE',  ( 0.5042675786779511338, 6.230788509548835563, 18.87331068310452054 ) ) ;
#1770 = CARTESIAN_POINT ( 'NONE',  ( 2.500000000000000444, 187.1499999978150868, 5.964466094067262247 ) ) ;
#1771 = CIRCLE ( 'NONE', #763, 1.000000000000000444 ) ;
#1772 = CARTESIAN_POINT ( 'NONE',  ( -1.035533905932737753, 184.9499999978150413, 4.500000000000001776 ) ) ;
#1773 = DIRECTION ( 'NONE',  ( 0.5877852522924802425, -0.8090169943749422332, 0.000000000000000000 ) ) ;
#1774 = CARTESIAN_POINT ( 'NONE',  ( 9.750000000000003553, 106.0000000000000142, 1.020968533498575461E-13 ) ) ;
#1775 = CARTESIAN_POINT ( 'NONE',  ( -5.317509234263930296, -2.779225709351048401, 5.000000000000004441 ) ) ;
#1776 = CARTESIAN_POINT ( 'NONE',  ( 2.255245247391631569, 227.9269692368775395, 9.203290779546277278 ) ) ;
#1777 = CARTESIAN_POINT ( 'NONE',  ( -1.979540121751099724, 226.5646310999674427, 5.192482286045976281 ) ) ;
#1778 = ORIENTED_EDGE ( 'NONE', *, *, #13016, .T. ) ;
#1779 = CARTESIAN_POINT ( 'NONE',  ( 4.005998022990028495, -4.467726698309201439, 4.200681937418260681 ) ) ;
#1780 = ORIENTED_EDGE ( 'NONE', *, *, #6602, .F. ) ;
#1781 = CARTESIAN_POINT ( 'NONE',  ( -2.817313151351311884, 5.579000502529369854, 17.86765874365829276 ) ) ;
#1782 = CARTESIAN_POINT ( 'NONE',  ( -2.500000000000000444, 189.0500374527063343, 5.965241810263807842 ) ) ;
#1783 = CARTESIAN_POINT ( 'NONE',  ( -4.196288036172577840, 4.288789315524710766, 23.99687951097622829 ) ) ;
#1784 = CARTESIAN_POINT ( 'NONE',  ( -0.8002302970946589822, 5.947135855825866457, 4.386017732123007384 ) ) ;
#1785 = CARTESIAN_POINT ( 'NONE',  ( 2.174380334507205248, 227.9547525935562646, 9.285006124859036092 ) ) ;
#1786 = B_SPLINE_CURVE_WITH_KNOTS ( 'NONE', 3,
 ( #13951, #14106, #5690, #15157, #8073, #11411, #10228, #3061, #7992, #10536, #15394, #9192, #12833, #12754, #9343, #13871, #14031, #590 ),
 .UNSPECIFIED., .F., .F.,
 ( 4, 2, 2, 2, 2, 2, 2, 2, 4 ),
 ( 0.003131486019301987691, 0.003522824630466695264, 0.003914163241631402404, 0.004305501852796110411, 0.004696840463960817551, 0.005088179075125525558, 0.005479517686290230963, 0.005870856297454938102, 0.006262194908619644375 ),
 .UNSPECIFIED. ) ;
#1787 = CARTESIAN_POINT ( 'NONE',  ( 4.344313232727111007, 4.493553492990106868, 5.504369696801527212 ) ) ;
#1788 = CARTESIAN_POINT ( 'NONE',  ( 2.500000000000000000, 3.061616997868383141E-16, 0.5000000000000000000 ) ) ;
#1789 = CARTESIAN_POINT ( 'NONE',  ( 0.000000000000000000, -0.3999999999999906408, -2.750000000000010658 ) ) ;
#1790 = CARTESIAN_POINT ( 'NONE',  ( -2.931156713028406635, -5.520271803279254819, 30.49563030319847101 ) ) ;
#1791 = CARTESIAN_POINT ( 'NONE',  ( 1.767766952966369320, 185.7000000000000171, 5.232233047033630235 ) ) ;
#1792 = CARTESIAN_POINT ( 'NONE',  ( -1.914314807121730633, 228.0813985855225212, 6.474474614426593888 ) ) ;
#1793 = PRODUCT_DEFINITION_CONTEXT ( 'detailed design', #15421, 'design' ) ;
#1794 = FACE_BOUND ( 'NONE', #1352, .T. ) ;
#1795 = CARTESIAN_POINT ( 'NONE',  ( -5.620879908643947154, 2.102487719021948642, 18.97377823943293151 ) ) ;
#1796 = CARTESIAN_POINT ( 'NONE',  ( 2.066987300000000083, -0.8561741729129450640, -1.599999998907525756 ) ) ;
#1797 = CARTESIAN_POINT ( 'NONE',  ( 2.500000000000000444, 185.6500000000000341, 5.964466094067262247 ) ) ;
#1798 = CARTESIAN_POINT ( 'NONE',  ( 2.841163418881286429, -5.567120626447985998, 24.76236973443873879 ) ) ;
#1800 = ORIENTED_EDGE ( 'NONE', *, *, #2729, .T. ) ;
#1799 = CARTESIAN_POINT ( 'NONE',  ( 2.066987299999999639, 186.7999999989075093, 7.856174172912946396 ) ) ;
#1801 = CARTESIAN_POINT ( 'NONE',  ( -3.311384659207173620, -5.004923837169396705, 17.02641404563305372 ) ) ;
#1802 = EDGE_CURVE ( 'NONE', #2728, #7333, #13264, .T. ) ;
#1803 = CARTESIAN_POINT ( 'NONE',  ( -0.9740012993920151851, -6.173846968979639804, 5.261649206284398694 ) ) ;
#1804 = EDGE_CURVE ( 'NONE', #5264, #3385, #3580, .T. ) ;
#1805 = CARTESIAN_POINT ( 'NONE',  ( -5.783239563508439041, 1.602707436861068313, 4.026414045633067929 ) ) ;
#1806 =( NAMED_UNIT ( * ) SI_UNIT ( $, .STERADIAN. ) SOLID_ANGLE_UNIT ( ) );
#1807 = CARTESIAN_POINT ( 'NONE',  ( 2.989629975077807256, 189.8928756713021357, 6.972882067819393015 ) ) ;
#1808 = B_SPLINE_CURVE_WITH_KNOTS ( 'NONE', 3,
 ( #5054, #9908, #14762, #7514, #1456, #6334, #11171, #5134, #11403, #15071, #350, #4086, #14022, #15222, #5215, #1541, #1692, #13789 ),
 .UNSPECIFIED., .F., .F.,
 ( 4, 2, 2, 2, 2, 2, 2, 2, 4 ),
 ( 0.000000000000000000, 0.0003914357524127486240, 0.0007828715048254972480, 0.001174307257238245980, 0.001565743009650994496, 0.001957178762063743228, 0.002348614514476492394, 0.002740050266889241994, 0.003131486019301991160 ),
 .UNSPECIFIED. ) ;
#1809 = CARTESIAN_POINT ( 'NONE',  ( -3.061616997868391523E-16, 189.0000000000000000, -7.000000000000000000 ) ) ;
#1810 = CARTESIAN_POINT ( 'NONE',  ( -0.8002302970946246763, 5.947135855825869122, 30.38601773212298340 ) ) ;
#1811 = CARTESIAN_POINT ( 'NONE',  ( 1.813601955701626300, 228.5298646585827385, 7.769670212251800656 ) ) ;
#1812 = CARTESIAN_POINT ( 'NONE',  ( -4.267838854167165685, 4.217593933790345417, 30.73760108194402463 ) ) ;
#1813 = CARTESIAN_POINT ( 'NONE',  ( -2.066987299999999639, 0.8561741729129455081, 2.200000001092474733 ) ) ;
#1814 = FACE_OUTER_BOUND ( 'NONE', #10483, .T. ) ;
#1815 = ORIENTED_EDGE ( 'NONE', *, *, #4228, .T. ) ;
#1816 = CARTESIAN_POINT ( 'NONE',  ( -5.285485590866834116E-16, 186.4499999989075150, 9.066987300000000971 ) ) ;
#1817 = ORIENTED_EDGE ( 'NONE', *, *, #9119, .F. ) ;
#1818 = CARTESIAN_POINT ( 'NONE',  ( -5.931734679891428108, 0.9039278060245400370, 24.76382603205594179 ) ) ;
#1819 =( REPRESENTATION_RELATIONSHIP ('NONE','NONE', #11191, #4596 ) REPRESENTATION_RELATIONSHIP_WITH_TRANSFORMATION ( #13691 )SHAPE_REPRESENTATION_RELATIONSHIP( ) );
#1820 = VERTEX_POINT ( 'NONE', #14701 ) ;
#1821 = CYLINDRICAL_SURFACE ( 'NONE', #14190, 0.9999999999999998890 ) ;
#1822 = CARTESIAN_POINT ( 'NONE',  ( -1.530808498934191571E-16, 2.500000000000000000, -3.199999997815050623 ) ) ;
#1823 = ADVANCED_FACE ( 'NONE', ( #12301 ), #7614, .T. ) ;
#1824 = AXIS2_PLACEMENT_3D ( 'NONE', #5870, #7799, #10718 ) ;
#1825 = CARTESIAN_POINT ( 'NONE',  ( 3.796994071234844259E-16, -2.066987299999999639, -2.549999998907525267 ) ) ;
#1826 =( BOUNDED_CURVE ( )  B_SPLINE_CURVE ( 2, ( #10332, #15186, #11209, #4283, #3089, #8836, #7632, #1499, #1653 ),
 .UNSPECIFIED., .F., .F. ) 
 B_SPLINE_CURVE_WITH_KNOTS ( ( 3, 2, 2, 2, 3 ),
 ( 0.5714285714285713969, 0.5892857142857143016, 0.6071428571428570953, 0.6250000000000000000, 0.6428571428571429047 ),
 .UNSPECIFIED. ) 
 CURVE ( )  GEOMETRIC_REPRESENTATION_ITEM ( )  RATIONAL_B_SPLINE_CURVE ( ( 1.000000000000000000, 0.9238795325112867385, 1.000000000000000000, 0.9238795325112867385, 1.000000000000000000, 0.9238795325112867385, 1.000000000000000000, 0.9238795325112867385, 1.000000000000000000 ) ) 
 REPRESENTATION_ITEM ( '' )  );
#1827 = CARTESIAN_POINT ( 'NONE',  ( -3.459447313391775136, -5.206669755181035697, 5.974000980233304503 ) ) ;
#1828 = CARTESIAN_POINT ( 'NONE',  ( -1.767766952966369098, 1.767766952966369098, 0.000000000000000000 ) ) ;
#1829 = CARTESIAN_POINT ( 'NONE',  ( 2.668367453516707233, -5.373994336898093138, 5.000000000000004441 ) ) ;
#1830 = CARTESIAN_POINT ( 'NONE',  ( -3.312341048453546932, 5.004306261885401952, 17.02601979877759319 ) ) ;
#1831 = CARTESIAN_POINT ( 'NONE',  ( -2.500000000000000444, 186.7999999999999829, 7.000000000000000000 ) ) ;
#1832 = CARTESIAN_POINT ( 'NONE',  ( 2.066987299999999639, 2.531329380823229670E-16, -2.149999998907525356 ) ) ;
#1833 = ORIENTED_EDGE ( 'NONE', *, *, #2892, .T. ) ;
#1834 = CIRCLE ( 'NONE', #816, 1.500000000000000000 ) ;
#1835 = ORIENTED_EDGE ( 'NONE', *, *, #12602, .T. ) ;
#1836 = ORIENTED_EDGE ( 'NONE', *, *, #6502, .T. ) ;
#1837 = B_SPLINE_CURVE_WITH_KNOTS ( 'NONE', 3,
 ( #10194, #15200, #11529, #5579, #1007, #15045, #1899, #11608, #12648, #10270, #13176, #9088, #5501, #9528, #1979, #628, #15277, #14364 ),
 .UNSPECIFIED., .F., .F.,
 ( 4, 2, 2, 2, 2, 2, 2, 2, 4 ),
 ( 0.003131918686235979094, 0.003523310662250268930, 0.003914702638264559199, 0.004306094614278849035, 0.004697486590293138871, 0.005088878566307429574, 0.005480270542321719410, 0.005871662518336009245, 0.006263054494350299081 ),
 .UNSPECIFIED. ) ;
#1838 = CARTESIAN_POINT ( 'NONE',  ( 2.817313151351127587, -5.579000502529462224, 11.49999999999998224 ) ) ;
#1839 = DIRECTION ( 'NONE',  ( -0.000000000000000000, -1.000000000000000000, -0.000000000000000000 ) ) ;
#1840 = EDGE_LOOP ( 'NONE', ( #5126, #1408 ) ) ;
#1841 = DIRECTION ( 'NONE',  ( -0.000000000000000000, 1.000000000000000000, -0.000000000000000000 ) ) ;
#1842 = CARTESIAN_POINT ( 'NONE',  ( 1.767766952966369320, -1.767766952966368654, 0.5000000021849494436 ) ) ;
#1843 = CARTESIAN_POINT ( 'NONE',  ( -5.317509234263865459, -2.779225709351170526, 17.99999999999998934 ) ) ;
#1844 = CARTESIAN_POINT ( 'NONE',  ( 1.767766952966368432, 187.7999999978150356, 8.767766952966368876 ) ) ;
#1845 = CARTESIAN_POINT ( 'NONE',  ( -1.035533905932739751, 189.2499999978150811, 9.500000000000003553 ) ) ;
#1846 = ADVANCED_FACE ( 'NONE', ( #14780 ), #13571, .F. ) ;
#1847 = CIRCLE ( 'NONE', #2630, 1.499999999999999556 ) ;
#1848 = CARTESIAN_POINT ( 'NONE',  ( -2.500000000000000000, -0.9567085809127248153, 2.553193976603714610 ) ) ;
#1849 = CARTESIAN_POINT ( 'NONE',  ( 5.487097279078465561, 2.429065649168737462, 18.79952054102714598 ) ) ;
#1850 = PRODUCT_CONTEXT ( 'NONE', #477, 'mechanical' ) ;
#1851 = CARTESIAN_POINT ( 'NONE',  ( -1.035533905932739751, 189.3199999975965682, 9.500000000000003553 ) ) ;
#1852 = CARTESIAN_POINT ( 'NONE',  ( -0.6401557763822781633, 228.8776351522889172, 8.774051233606112277 ) ) ;
#1853 = EDGE_CURVE ( 'NONE', #3437, #2475, #6220, .T. ) ;
#1854 = CARTESIAN_POINT ( 'NONE',  ( 5.131373506000599605, 7.062729720844090231, 5.000000000000004441 ) ) ;
#1855 = B_SPLINE_CURVE_WITH_KNOTS ( 'NONE', 3,
 ( #6718, #15218, #4318, #4473, #9565, #15377, #13133, #12974, #10676, #4714, #8058, #13219, #809, #14170, #9327, #9255, #3275, #8138 ),
 .UNSPECIFIED., .F., .F.,
 ( 4, 2, 2, 2, 2, 2, 2, 2, 4 ),
 ( 0.000000000000000000, 0.0003914898357794973868, 0.0007829796715589947735, 0.001174469507338492215, 0.001565959343117989547, 0.001957449178897487096, 0.002348939014676984429, 0.002740428850456481762, 0.003131918686235979094 ),
 .UNSPECIFIED. ) ;
#1856 = ORIENTED_EDGE ( 'NONE', *, *, #9485, .T. ) ;
#1857 = CARTESIAN_POINT ( 'NONE',  ( -1.798270642782740181, 1.742470094454686036, -2.500251818840280471 ) ) ;
#1858 = VECTOR ( 'NONE', #12170, 1000.000000000000000 ) ;
#1859 = ORIENTED_EDGE ( 'NONE', *, *, #3113, .F. ) ;
#1860 = CARTESIAN_POINT ( 'NONE',  ( -0.5039005892420553856, 6.230833003620545263, 10.62636388911295882 ) ) ;
#1861 = DIRECTION ( 'NONE',  ( 0.000000000000000000, 0.000000000000000000, 1.000000000000000000 ) ) ;
#1862 = PLANE ( 'NONE',  #13441 ) ;
#1863 = DIRECTION ( 'NONE',  ( -0.3090169943749447867, -0.9510565162951544194, 0.000000000000000000 ) ) ;
#1864 = LINE ( 'NONE', #3218, #4114 ) ;
#1865 = CARTESIAN_POINT ( 'NONE',  ( 1.035533905932739085, -2.500000000000000000, 1.949999999999999956 ) ) ;
#1866 = CARTESIAN_POINT ( 'NONE',  ( -1.767766952966368432, -1.767766952966369320, -1.400000000000000133 ) ) ;
#1867 = CARTESIAN_POINT ( 'NONE',  ( 4.286401442266532413, 4.198423832313196158, 4.867639214160894845 ) ) ;
#1868 = CIRCLE ( 'NONE', #9765, 1.499999999999999556 ) ;
#1869 = CARTESIAN_POINT ( 'NONE',  ( 0.02899383802118515874, 0.4000000000000097367, -2.522283165497673618 ) ) ;
#1870 = CARTESIAN_POINT ( 'NONE',  ( -1.035533905932739529, 186.0499999978150356, 9.500000000000003553 ) ) ;
#1871 = CARTESIAN_POINT ( 'NONE',  ( 0.5489208960863538600, 227.6341400683239726, 5.182766506802777506 ) ) ;
#1872 = CARTESIAN_POINT ( 'NONE',  ( 0.000000000000000000, 0.000000000000000000, 53.67766952966368876 ) ) ;
#1873 = CARTESIAN_POINT ( 'NONE',  ( 0.6144300524836082689, 6.220417338033028543, 23.70033372175935682 ) ) ;
#1874 = CARTESIAN_POINT ( 'NONE',  ( 0.8561741729129452860, 2.066987299999999639, -2.199999998907525622 ) ) ;
#1875 = CARTESIAN_POINT ( 'NONE',  ( -1.035533905932737975, 185.8500000000000227, 4.500000000000000888 ) ) ;
#1876 = CARTESIAN_POINT ( 'NONE',  ( -4.070051655338261298, 4.744673454622341247, 25.37367328635991370 ) ) ;
#1878 = ORIENTED_EDGE ( 'NONE', *, *, #2692, .F. ) ;
#1877 = CARTESIAN_POINT ( 'NONE',  ( -0.9999196734180613166, -5.916093360767550102, 24.36725955955066780 ) ) ;
#1879 = CARTESIAN_POINT ( 'NONE',  ( 0.5662760513513176441, 0.4000000000000062395, 2.593905796087985216 ) ) ;
#1880 = CARTESIAN_POINT ( 'NONE',  ( 5.531757352715644060, -2.326874507723228458, 17.12619317285288645 ) ) ;
#1881 = AXIS2_PLACEMENT_3D ( 'NONE', #7229, #12222, #14622 ) ;
#1882 = CYLINDRICAL_SURFACE ( 'NONE', #12144, 1.499999999999999556 ) ;
#1883 = CARTESIAN_POINT ( 'NONE',  ( -1.898822140593172669, 189.7510425599547261, 9.704729509603533089 ) ) ;
#1884 = PRESENTATION_STYLE_ASSIGNMENT (( #12780 ) ) ;
#1885 = DIRECTION ( 'NONE',  ( -0.000000000000000000, 1.000000000000000000, -0.000000000000000000 ) ) ;
#1886 = CARTESIAN_POINT ( 'NONE',  ( -4.912791094074941967E-16, 184.5300000002184788, 9.500000000000001776 ) ) ;
#1887 = DIRECTION ( 'NONE',  ( 0.000000000000000000, 0.000000000000000000, -1.000000000000000000 ) ) ;
#1888 = CARTESIAN_POINT ( 'NONE',  ( 0.06495987523896813720, 228.9118724015956730, 8.872930362369002566 ) ) ;
#1889 = CARTESIAN_POINT ( 'NONE',  ( 7.180990026460747799, -3.384707322287378695, 31.00000000000000000 ) ) ;
#1890 = CARTESIAN_POINT ( 'NONE',  ( 0.04799661009841083015, 0.4000000000000045186, 2.537470117151901405 ) ) ;
#1891 = DIRECTION ( 'NONE',  ( 0.000000000000000000, 0.000000000000000000, 1.000000000000000000 ) ) ;
#1892 = EDGE_LOOP ( 'NONE', ( #8151, #8211, #9561, #6789 ) ) ;
#1893 = CARTESIAN_POINT ( 'NONE',  ( 1.461580736456473462, 185.1499999989075320, 5.538419263543526760 ) ) ;
#1894 = EDGE_CURVE ( 'NONE', #1004, #3420, #14147, .T. ) ;
#1895 = CARTESIAN_POINT ( 'NONE',  ( 2.500000000000000444, 184.7500000000000000, 8.035533905932739529 ) ) ;
#1896 = AXIS2_PLACEMENT_3D ( 'NONE', #10725, #15583, #14373 ) ;
#1897 = VERTEX_POINT ( 'NONE', #5154 ) ;
#1898 = DIRECTION ( 'NONE',  ( -1.000000000000000000, 0.000000000000000000, 0.000000000000000000 ) ) ;
#1899 = CARTESIAN_POINT ( 'NONE',  ( -5.531209434046322926, -2.328189801702654549, 30.12696220972948424 ) ) ;
#1900 = CARTESIAN_POINT ( 'NONE',  ( -2.066987300000000083, 184.7999999989075093, 6.143825827087054492 ) ) ;
#1901 = CARTESIAN_POINT ( 'NONE',  ( 5.620786884546309814, 2.102685372472837599, 17.02641404563306082 ) ) ;
#1902 = CARTESIAN_POINT ( 'NONE',  ( -2.066987300000000527, 184.6499999989075320, 7.000000000000000000 ) ) ;
#1903 = CARTESIAN_POINT ( 'NONE',  ( 5.903230462362999198, -1.077253041748644558, 23.88557478428062097 ) ) ;
#1904 = CARTESIAN_POINT ( 'NONE',  ( -1.767766952966368432, -1.767766952966369320, -0.6000000000000003109 ) ) ;
#1905 = CARTESIAN_POINT ( 'NONE',  ( 2.500000000000000444, -1.035533905932737309, -1.149999999999999689 ) ) ;
#1906 = VECTOR ( 'NONE', #7020, 1000.000000000000000 ) ;
#1907 = CARTESIAN_POINT ( 'NONE',  ( 0.000000000000000000, 201.6409668649146738, 13.30942870683726298 ) ) ;
#1908 = AXIS2_PLACEMENT_3D ( 'NONE', #3067, #5542, #5467 ) ;
#1909 = FACE_OUTER_BOUND ( 'NONE', #122, .T. ) ;
#1910 = CARTESIAN_POINT ( 'NONE',  ( -5.620879908643915179, -2.102487719022031243, 17.02622176056705783 ) ) ;
#1911 = CARTESIAN_POINT ( 'NONE',  ( -0.9999196734181325930, -5.916093360767538556, 17.86725955955069978 ) ) ;
#1912 = EDGE_CURVE ( 'NONE', #2813, #6711, #6038, .T. ) ;
#1913 = ORIENTED_EDGE ( 'NONE', *, *, #792, .F. ) ;
#1914 = ORIENTED_EDGE ( 'NONE', *, *, #2090, .T. ) ;
#1915 = EDGE_LOOP ( 'NONE', ( #1624, #4932, #12716, #2964 ) ) ;
#1916 = CARTESIAN_POINT ( 'NONE',  ( -6.155854678529464330, -1.081900940642162690, 10.99574050496990196 ) ) ;
#1917 = FACE_OUTER_BOUND ( 'NONE', #13307, .T. ) ;
#1918 = ADVANCED_FACE ( 'NONE', ( #292, #10009, #1323, #4025, #14855, #8817, #13646, #8901, #4999, #2762, #12460, #11270, #2844, #7690, #370, #5237, #10083, #14933, #14624, #6724, #4923, #3713, #8589, #13424, #2527, #7383 ), #12224, .T. ) ;
#1919 = ORIENTED_EDGE ( 'NONE', *, *, #13965, .F. ) ;
#1920 = CARTESIAN_POINT ( 'NONE',  ( 5.782895619916205376, -1.604017620857909998, 18.97408052783099563 ) ) ;
#1921 = CARTESIAN_POINT ( 'NONE',  ( 1.767766952966369320, -1.767766952966368654, -0.2999999978150506563 ) ) ;
#1922 = CARTESIAN_POINT ( 'NONE',  ( -0.5043776560896956473, 6.230795654995843869, 18.87337476296005079 ) ) ;
#1923 = CARTESIAN_POINT ( 'NONE',  ( 3.159612573729055907, 5.393342049074733247, 25.30026515017675948 ) ) ;
#1924 = CARTESIAN_POINT ( 'NONE',  ( 2.500000000000000000, 188.6499999978150584, 8.035533905932739529 ) ) ;
#1925 = CARTESIAN_POINT ( 'NONE',  ( -1.035533905932738197, -2.500000000000000000, 1.856999999978150573 ) ) ;
#1926 = DIRECTION ( 'NONE',  ( 0.9510565162951499785, 0.3090169943749582204, 0.000000000000000000 ) ) ;
#1927 = APPLICATION_PROTOCOL_DEFINITION ( 'draft international standard', 'automotive_design', 1998, #13696 ) ;
#1928 = CARTESIAN_POINT ( 'NONE',  ( -0.8561741729129455081, 2.066987299999999639, 0.3000000010924747662 ) ) ;
#1929 = CARTESIAN_POINT ( 'NONE',  ( -1.524659305057740610E-16, 188.9699999975965738, 4.500000000000000000 ) ) ;
#1930 = CARTESIAN_POINT ( 'NONE',  ( -1.864336199031810581, 228.4898043637318779, 7.653973795834509097 ) ) ;
#1931 = CYLINDRICAL_SURFACE ( 'NONE', #4961, 1.499999999999999556 ) ;
#1932 = ORIENTED_EDGE ( 'NONE', *, *, #7820, .F. ) ;
#1933 = CARTESIAN_POINT ( 'NONE',  ( 2.383412885783723123, 0.8083228232074107789, -2.500305643928210309 ) ) ;
#1934 = EDGE_CURVE ( 'NONE', #8231, #10984, #6388, .T. ) ;
#1935 = ORIENTED_EDGE ( 'NONE', *, *, #4528, .T. ) ;
#1936 = CARTESIAN_POINT ( 'NONE',  ( -4.344762547369822592, 4.493114738039108325, 17.49691356133953590 ) ) ;
#1937 = DIRECTION ( 'NONE',  ( 0.000000000000000000, 0.000000000000000000, 1.000000000000000000 ) ) ;
#1938 = CARTESIAN_POINT ( 'NONE',  ( -0.6152055445546463774, 5.969096820685154015, 5.799049686702669071 ) ) ;
#1939 = ORIENTED_EDGE ( 'NONE', *, *, #7499, .F. ) ;
#1940 = B_SPLINE_CURVE_WITH_KNOTS ( 'NONE', 3,
 ( #3323, #15424, #9455, #9536, #8025, #11908, #14290, #2123, #9226, #10802, #11754, #8187, #2284, #11990, #8109, #14059, #13024, #7072 ),
 .UNSPECIFIED., .F., .F.,
 ( 4, 2, 2, 2, 2, 2, 2, 2, 4 ),
 ( 0.000000000000000000, 0.0003914357524127449377, 0.0007828715048254898754, 0.001174307257238234922, 0.001565743009650979751, 0.001957178762063724580, 0.002348614514476469843, 0.002740050266889214672, 0.003131486019301959502 ),
 .UNSPECIFIED. ) ;
#1941 = CARTESIAN_POINT ( 'NONE',  ( -2.500000000000000000, 0.000000000000000000, 2.500000000000000000 ) ) ;
#1942 = CARTESIAN_POINT ( 'NONE',  ( 0.6543697108982007293, 2.434931691670788823, -2.500000000000000000 ) ) ;
#1943 = CARTESIAN_POINT ( 'NONE',  ( -1.530808498934191571E-16, 2.500000000000000000, -1.700000000000000622 ) ) ;
#1944 = CYLINDRICAL_SURFACE ( 'NONE', #14809, 2.500000000000000444 ) ;
#1945 =( LENGTH_UNIT ( ) NAMED_UNIT ( * ) SI_UNIT ( .MILLI., .METRE. ) );
#1946 = CARTESIAN_POINT ( 'NONE',  ( 7.799024015210631156, -1.482594289697088730, 5.000000000000004441 ) ) ;
#1947 = PRODUCT_DEFINITION_SHAPE ( 'NONE', 'NONE',  #15767 ) ;
#1948 =( BOUNDED_CURVE ( )  B_SPLINE_CURVE ( 2, ( #4139, #9162, #326, #13686, #7882, #10196, #3976, #2716, #13841 ),
 .UNSPECIFIED., .F., .F. ) 
 B_SPLINE_CURVE_WITH_KNOTS ( ( 3, 2, 2, 2, 3 ),
 ( 0.7142857142857143016, 0.7321428571428570953, 0.7500000000000000000, 0.7678571428571429047, 0.7857142857142856984 ),
 .UNSPECIFIED. ) 
 CURVE ( )  GEOMETRIC_REPRESENTATION_ITEM ( )  RATIONAL_B_SPLINE_CURVE ( ( 1.000000000000000000, 0.9238795325112867385, 1.000000000000000000, 0.9238795325112867385, 1.000000000000000000, 0.9238795325112867385, 1.000000000000000000, 0.9238795325112867385, 1.000000000000000000 ) ) 
 REPRESENTATION_ITEM ( '' )  );
#1949 = CARTESIAN_POINT ( 'NONE',  ( 1.767766952966368654, 185.3999999978150584, 8.767766952966368876 ) ) ;
#1950 = CARTESIAN_POINT ( 'NONE',  ( -1.990689658724532629, 228.2709309767465697, 7.021854970500988280 ) ) ;
#1951 = CYLINDRICAL_SURFACE ( 'NONE', #5267, 1.499999999999999556 ) ;
#1952 = DIRECTION ( 'NONE',  ( 0.000000000000000000, 0.000000000000000000, 1.000000000000000000 ) ) ;
#1953 = CARTESIAN_POINT ( 'NONE',  ( -2.066987299999999195, -0.8561741729129467293, -2.699999998907525178 ) ) ;
#1954 = CARTESIAN_POINT ( 'NONE',  ( -2.500000000000000444, 186.7999999999999829, 7.000000000000000000 ) ) ;
#1955 = CARTESIAN_POINT ( 'NONE',  ( 3.458623254138621483, -5.207221900902879952, 25.47377282875268278 ) ) ;
#1957 = ORIENTED_EDGE ( 'NONE', *, *, #12525, .T. ) ;
#1956 = CARTESIAN_POINT ( 'NONE',  ( 0.000000000000000000, 0.000000000000000000, 0.000000000000000000 ) ) ;
#1958 = LINE ( 'NONE', #9216, #11943 ) ;
#1959 = AXIS2_PLACEMENT_3D ( 'NONE', #1774, #8883, #6647 ) ;
#1960 = CIRCLE ( 'NONE', #5291, 1.499999999999999556 ) ;
#1961 = CARTESIAN_POINT ( 'NONE',  ( -5.375763363753385704, 2.665284979407666732, 23.99610204984015382 ) ) ;
#1962 = CARTESIAN_POINT ( 'NONE',  ( -2.977464457213339077, 189.8978568417799693, 6.866500699578031330 ) ) ;
#1963 = CARTESIAN_POINT ( 'NONE',  ( 0.07162629256299407610, 188.9999999999999716, 4.501026275805653398 ) ) ;
#1964 = CARTESIAN_POINT ( 'NONE',  ( -1.767766952966369098, 185.0300000002184788, 5.232233047033630235 ) ) ;
#1965 = CARTESIAN_POINT ( 'NONE',  ( -1.739397458836472676, 227.9323402172746853, 6.043985545194606956 ) ) ;
#1966 = CARTESIAN_POINT ( 'NONE',  ( 1.923823996436629047, 228.4292023995385250, 7.478951866735841669 ) ) ;
#1967 = FACE_BOUND ( 'NONE', #9173, .T. ) ;
#1968 = CARTESIAN_POINT ( 'NONE',  ( 1.511918676366796888E-05, 0.4000000000000080158, 2.452725668627568023 ) ) ;
#1969 = CARTESIAN_POINT ( 'NONE',  ( 1.035533905932739085, -2.500000000000000000, 1.250000002184949999 ) ) ;
#1970 = ORIENTED_EDGE ( 'NONE', *, *, #9346, .T. ) ;
#1971 = CARTESIAN_POINT ( 'NONE',  ( -1.461580736456473906, 186.3499999989074922, 8.461580736456474128 ) ) ;
#1972 = CIRCLE ( 'NONE', #6060, 5.000000000000000000 ) ;
#1973 = CARTESIAN_POINT ( 'NONE',  ( -1.035533905932739529, 184.5499999999999829, 9.500000000000000000 ) ) ;
#1974 = AXIS2_PLACEMENT_3D ( 'NONE', #8448, #2622, #7478 ) ;
#1975 = CARTESIAN_POINT ( 'NONE',  ( 5.375886393124376994, -2.665038680141303740, 5.504397606442131163 ) ) ;
#1976 = EDGE_CURVE ( 'NONE', #15372, #15063, #4775, .T. ) ;
#1977 = ORIENTED_EDGE ( 'NONE', *, *, #6193, .F. ) ;
#1978 = CYLINDRICAL_SURFACE ( 'NONE', #8634, 1.000000000000000444 ) ;
#1979 = CARTESIAN_POINT ( 'NONE',  ( -5.915641100987819812, -1.003868594704814932, 30.49571079637979665 ) ) ;
#1980 = CARTESIAN_POINT ( 'NONE',  ( -3.922672396097092840, 4.541739265057668007, 31.87364704684421923 ) ) ;
#1981 = DIRECTION ( 'NONE',  ( 0.000000000000000000, 0.000000000000000000, 1.000000000000000000 ) ) ;
#1982 = CARTESIAN_POINT ( 'NONE',  ( 1.461580736456472795, 184.9499999989075150, 8.461580736456474128 ) ) ;
#1983 = VECTOR ( 'NONE', #1839, 1000.000000000000000 ) ;
#1984 = CARTESIAN_POINT ( 'NONE',  ( -0.9740856415298599913, 6.173834621338629702, 24.23852653055524442 ) ) ;
#1985 = CARTESIAN_POINT ( 'NONE',  ( 1.035533905932737531, 2.500000000000000444, -0.04999999781505021224 ) ) ;
#1986 = CARTESIAN_POINT ( 'NONE',  ( 9.750000000000003553, 22.00000000000000000, 1.020968533498575335E-13 ) ) ;
#1987 = CARTESIAN_POINT ( 'NONE',  ( 5.999999999999999112, 221.4150671951173592, 6.196499129422101682 ) ) ;
#1988 = CARTESIAN_POINT ( 'NONE',  ( -5.570722351696168140, -2.834100162822159596, 24.76190213084012370 ) ) ;
#1989 = CARTESIAN_POINT ( 'NONE',  ( -5.866923913994614104, -1.260079467906668027, 17.20047945897285047 ) ) ;
#1990 = LINE ( 'NONE', #7015, #12015 ) ;
#1991 = ORIENTED_EDGE ( 'NONE', *, *, #14241, .F. ) ;
#1992 = ORIENTED_EDGE ( 'NONE', *, *, #488, .T. ) ;
#1993 = ORIENTED_EDGE ( 'NONE', *, *, #6351, .T. ) ;
#1994 = CARTESIAN_POINT ( 'NONE',  ( 2.930600586412925868, -5.520563544161773528, 18.50308643866044633 ) ) ;
#1995 = CARTESIAN_POINT ( 'NONE',  ( 3.659182332138073087E-16, 190.0875178197511275, 4.201689379953569947 ) ) ;
#1996 = ORIENTED_EDGE ( 'NONE', *, *, #1610, .T. ) ;
#1997 = CARTESIAN_POINT ( 'NONE',  ( 9.750000000000003553, 184.0000000000000000, 1.020968533498575461E-13 ) ) ;
#1998 = CARTESIAN_POINT ( 'NONE',  ( 1.767766952966368654, 1.767766952966369098, -0.09999999781505033991 ) ) ;
#1999 = EDGE_CURVE ( 'NONE', #7891, #6928, #9713, .T. ) ;
#2000 = CARTESIAN_POINT ( 'NONE',  ( -0.1306497350715297157, 6.000000000000007105, 23.50000000000000000 ) ) ;
#2001 = DIRECTION ( 'NONE',  ( 0.000000000000000000, 0.000000000000000000, 1.000000000000000000 ) ) ;
#2002 = CARTESIAN_POINT ( 'NONE',  ( -1.461580736456473240, 184.9499999989075150, 8.461580736456472351 ) ) ;
#2003 = CARTESIAN_POINT ( 'NONE',  ( -1.035533905932738197, -2.500000000000000000, -0.5430000000218496714 ) ) ;
#2004 = EDGE_CURVE ( 'NONE', #15509, #10326, #146, .T. ) ;
#2005 = CARTESIAN_POINT ( 'NONE',  ( 2.283493650000000486, 184.1249999994537632, 7.000000000000000000 ) ) ;
#2006 = ITEM_DEFINED_TRANSFORMATION ( 'NONE', 'NONE', #2026,  #14201 ) ;
#2007 = CARTESIAN_POINT ( 'NONE',  ( 1.461580736456472573, 1.461580736456472795, 0.9500000010924747329 ) ) ;
#2008 = CARTESIAN_POINT ( 'NONE',  ( -5.746996058422766396, -1.729015645941953672, 3.999920388255239434 ) ) ;
#2009 = CARTESIAN_POINT ( 'NONE',  ( 2.809728313654571430, 226.9499418402095046, 6.327683296853605199 ) ) ;
#2010 = ADVANCED_FACE ( 'NONE', ( #9631 ), #10356, .T. ) ;
#2011 = CARTESIAN_POINT ( 'NONE',  ( -2.500000000000000444, 1.035533905932737753, 0.9500000021849498433 ) ) ;
#2012 = VERTEX_POINT ( 'NONE', #2212 ) ;
#2013 = CARTESIAN_POINT ( 'NONE',  ( 4.142173849413810949, -4.341773579105344893, 4.384806175511481996 ) ) ;
#2014 = ORIENTED_EDGE ( 'NONE', *, *, #3349, .T. ) ;
#2015 = CARTESIAN_POINT ( 'NONE',  ( -4.290821322214496192, 4.545321419741441105, 17.38558052754515160 ) ) ;
#2016 = DIRECTION ( 'NONE',  ( 0.5877852522924802425, -0.8090169943749422332, 0.000000000000000000 ) ) ;
#2017 = CYLINDRICAL_SURFACE ( 'NONE', #8633, 7.000000000000000000 ) ;
#2018 = ORIENTED_EDGE ( 'NONE', *, *, #1640, .F. ) ;
#2019 = CARTESIAN_POINT ( 'NONE',  ( 4.416397290909871209, 4.422724436066468812, 11.23620383159194702 ) ) ;
#2020 = LINE ( 'NONE', #10465, #6923 ) ;
#2021 = CYLINDRICAL_SURFACE ( 'NONE', #1908, 12.49999999999999822 ) ;
#2022 = CARTESIAN_POINT ( 'NONE',  ( 2.500000000000000444, 1.035533905932737975, -0.2500000000000002220 ) ) ;
#2023 = PLANE ( 'NONE',  #12768 ) ;
#2024 = CARTESIAN_POINT ( 'NONE',  ( 0.009304900478233046543, 0.4000000000000027978, -2.495165599816074664 ) ) ;
#2025 = CARTESIAN_POINT ( 'NONE',  ( 1.035533905932738197, 187.8500000000000227, 9.500000000000003553 ) ) ;
#2027 = CARTESIAN_POINT ( 'NONE',  ( -1.964265005259087538, 228.3667458257928047, 7.298573719466742382 ) ) ;
#2026 = AXIS2_PLACEMENT_3D ( 'NONE', #15561, #6899, #4663 ) ;
#2028 = CARTESIAN_POINT ( 'NONE',  ( 6.021135683317733189, -1.680226122398085220, 17.02622717124729945 ) ) ;
#2029 =( BOUNDED_CURVE ( )  B_SPLINE_CURVE ( 2, ( #2982, #4095, #13795, #5610, #10458, #4413, #6575, #14103, #2904 ),
 .UNSPECIFIED., .F., .F. ) 
 B_SPLINE_CURVE_WITH_KNOTS ( ( 3, 2, 2, 2, 3 ),
 ( 0.2142857142857142738, 0.2321428571428571508, 0.2500000000000000000, 0.2678571428571428492, 0.2857142857142856984 ),
 .UNSPECIFIED. ) 
 CURVE ( )  GEOMETRIC_REPRESENTATION_ITEM ( )  RATIONAL_B_SPLINE_CURVE ( ( 1.000000000000000000, 0.9238795325112867385, 1.000000000000000000, 0.9238795325112867385, 1.000000000000000000, 0.9238795325112867385, 1.000000000000000000, 0.9238795325112867385, 1.000000000000000000 ) ) 
 REPRESENTATION_ITEM ( '' )  );
#2030 = CARTESIAN_POINT ( 'NONE',  ( 1.353717517954364224E-13, -6.250000000000000888, 18.99999999999998934 ) ) ;
#2031 = CARTESIAN_POINT ( 'NONE',  ( -2.066987299999999195, -0.8561741729129467293, -1.899999998907525800 ) ) ;
#2032 = CARTESIAN_POINT ( 'NONE',  ( -5.421010862427522170E-17, 187.4000000000000057, 4.500000000000000000 ) ) ;
#2033 = CARTESIAN_POINT ( 'NONE',  ( 7.000000000000006217, 1.500000000000008216, -8.673617379884158732E-16 ) ) ;
#2035 = VERTEX_POINT ( 'NONE', #11918 ) ;
#2034 = DIRECTION ( 'NONE',  ( 0.000000000000000000, 0.000000000000000000, 1.000000000000000000 ) ) ;
#2036 = EDGE_CURVE ( 'NONE', #7505, #5259, #3571, .T. ) ;
#2037 = CARTESIAN_POINT ( 'NONE',  ( 2.897581130414634077E-17, 19.99999999999999645, 9.750000000000003553 ) ) ;
#2038 = ORIENTED_EDGE ( 'NONE', *, *, #13999, .F. ) ;
#2039 = CARTESIAN_POINT ( 'NONE',  ( -5.746837578675966896, 1.729433780394384446, 23.50004946353776702 ) ) ;
#2040 = CARTESIAN_POINT ( 'NONE',  ( -3.000003100478683571, 227.2950289990915564, 7.343811503137294139 ) ) ;
#2041 =( LENGTH_UNIT ( ) NAMED_UNIT ( * ) SI_UNIT ( .MILLI., .METRE. ) );
#2042 = ADVANCED_FACE ( 'NONE', ( #4696, #8441 ), #7322, .F. ) ;
#2043 = CARTESIAN_POINT ( 'NONE',  ( 5.985119669071150561, 1.805077827356446507, 25.49991741810288559 ) ) ;
#2044 = CARTESIAN_POINT ( 'NONE',  ( 9.486769009248163798E-17, 184.9300000002185129, 4.500000000000000000 ) ) ;
#2045 = CARTESIAN_POINT ( 'NONE',  ( -1.926973947205288917, 228.4293926868652136, 7.479501427387623913 ) ) ;
#2046 = CARTESIAN_POINT ( 'NONE',  ( 1.498060502294345175, 227.8308734224802095, 5.750943654540091821 ) ) ;
#2047 = CARTESIAN_POINT ( 'NONE',  ( -2.668367453516725885, 5.373994336898083368, 31.00000000000000000 ) ) ;
#2048 = CARTESIAN_POINT ( 'NONE',  ( -5.558508435838230177, 2.857531096718855412, 4.869360672457871075 ) ) ;
#2049 = CARTESIAN_POINT ( 'NONE',  ( 5.131373506000437068, 7.062729720844210135, 24.49999999999999289 ) ) ;
#2050 = ORIENTED_EDGE ( 'NONE', *, *, #201, .T. ) ;
#2051 = CARTESIAN_POINT ( 'NONE',  ( -2.066987300000000971, 188.7999999989075093, 6.143825827087054492 ) ) ;
#2052 = B_SPLINE_CURVE_WITH_KNOTS ( 'NONE', 3,
 ( #1452, #2503, #4977, #13393, #9754, #6174, #3917, #7433, #10935, #6330, #8795, #268, #8488, #1222, #9982, #2418, #13623, #5130 ),
 .UNSPECIFIED., .F., .F.,
 ( 4, 2, 2, 2, 2, 2, 2, 2, 4 ),
 ( 0.000000000000000000, 0.0003914357524127467266, 0.0007828715048254934533, 0.001174307257238240126, 0.001565743009650986907, 0.001957178762063733687, 0.002348614514476480251, 0.002740050266889227249, 0.003131486019301973813 ),
 .UNSPECIFIED. ) ;
#2053 = CARTESIAN_POINT ( 'NONE',  ( 6.768587589771821120E-14, 6.000000000000000888, 12.49999999999998401 ) ) ;
#2054 = VERTEX_POINT ( 'NONE', #13437 ) ;
#2055 = CARTESIAN_POINT ( 'NONE',  ( -4.267992336621131422, -4.217442018460069164, 4.738056759968542586 ) ) ;
#2056 = CARTESIAN_POINT ( 'NONE',  ( 2.066987300000000083, 185.2999999989075377, 6.143825827087054492 ) ) ;
#2057 = CYLINDRICAL_SURFACE ( 'NONE', #5024, 2.499999999999999556 ) ;
#2058 = CARTESIAN_POINT ( 'NONE',  ( 2.066987300000000527, 187.4999999989075263, 6.143825827087054492 ) ) ;
#2059 = CARTESIAN_POINT ( 'NONE',  ( -3.883588957979163592, -4.898466244119004998, 5.973772828752684561 ) ) ;
#2060 = CARTESIAN_POINT ( 'NONE',  ( -1.035533905932737753, 2.500000000000000444, 0.8500000021849498655 ) ) ;
#2061 = CARTESIAN_POINT ( 'NONE',  ( 2.782468714962387235, -5.316055268221427710, 10.99610204984017336 ) ) ;
#2062 = B_SPLINE_CURVE_WITH_KNOTS ( 'NONE', 3,
 ( #7636, #8840, #3888, #10029, #388, #12560, #11291, #5258 ),
 .UNSPECIFIED., .F., .F.,
 ( 4, 2, 2, 4 ),
 ( 0.7729134150304844963, 0.8008314270218360731, 0.8287494390131875388, 0.8845854629958906923 ),
 .UNSPECIFIED. ) ;
#2063 = CARTESIAN_POINT ( 'NONE',  ( 0.000000000000000000, 201.6409668649146738, 13.30942870683726298 ) ) ;
#2064 = CARTESIAN_POINT ( 'NONE',  ( 1.767766952966369320, -1.767766952966368654, 1.199999999999999956 ) ) ;
#2065 = EDGE_CURVE ( 'NONE', #3287, #3420, #10896, .T. ) ;
#2066 = CARTESIAN_POINT ( 'NONE',  ( 3.779681992289790404, 4.979315417303903146, 31.99995078984292007 ) ) ;
#2067 = FACE_BOUND ( 'NONE', #14789, .T. ) ;
#2068 = ORIENTED_EDGE ( 'NONE', *, *, #12918, .F. ) ;
#2069 = ORIENTED_EDGE ( 'NONE', *, *, #4392, .T. ) ;
#2070 = ORIENTED_EDGE ( 'NONE', *, *, #652, .F. ) ;
#2071 = AXIS2_PLACEMENT_3D ( 'NONE', #15163, #5148, #1473 ) ;
#2072 = CARTESIAN_POINT ( 'NONE',  ( 0.8561741729129455081, 186.1999999989075150, 4.933012699999999029 ) ) ;
#2073 = CARTESIAN_POINT ( 'NONE',  ( -2.668367453516768517, 5.373994336898063828, 11.63239388001634822 ) ) ;
#2074 = ORIENTED_EDGE ( 'NONE', *, *, #10232, .F. ) ;
#2075 = PRODUCT_DEFINITION_SHAPE ( 'NONE', 'NONE',  #15748 ) ;
#2076 = CARTESIAN_POINT ( 'NONE',  ( 1.767766952966369320, -1.767766952966368654, 1.300000002184949599 ) ) ;
#2077 = CARTESIAN_POINT ( 'NONE',  ( 0.2622916576876685446, -5.995491482261829042, 5.973849426468138546 ) ) ;
#2078 = CARTESIAN_POINT ( 'NONE',  ( -3.779082820360602835, -4.979770177899319528, 3.999950931234675711 ) ) ;
#2079 = CARTESIAN_POINT ( 'NONE',  ( 0.8561741729129456191, 184.5999999989075206, 4.933012699999999029 ) ) ;
#2080 = CARTESIAN_POINT ( 'NONE',  ( 1.767766952966369320, -1.767766952966368654, 0.4069999999781502842 ) ) ;
#2081 = CARTESIAN_POINT ( 'NONE',  ( -2.668367453516708565, 5.373994336898094026, 5.000000000000004441 ) ) ;
#2082 = CARTESIAN_POINT ( 'NONE',  ( 1.767766952966369098, 188.8999999999999773, 5.232233047033630235 ) ) ;
#2083 = VECTOR ( 'NONE', #3978, 1000.000000000000000 ) ;
#2084 = CARTESIAN_POINT ( 'NONE',  ( -5.375605342016492649, -2.665598297262314897, 4.496879510976233618 ) ) ;
#2085 = CARTESIAN_POINT ( 'NONE',  ( 0.8272382227408706656, 226.3624115040579738, 4.596429122765971265 ) ) ;
#2086 = FACE_OUTER_BOUND ( 'NONE', #6484, .T. ) ;
#2087 = VERTEX_POINT ( 'NONE', #10735 ) ;
#2088 = LINE ( 'NONE', #14505, #10875 ) ;
#2089 = VERTEX_POINT ( 'NONE', #12160 ) ;
#2090 = EDGE_CURVE ( 'NONE', #12192, #1426, #8671, .T. ) ;
#2091 = CARTESIAN_POINT ( 'NONE',  ( -0.8736772044959224548, 6.188841968496069157, 10.99611573292808764 ) ) ;
#2092 = DIRECTION ( 'NONE',  ( 0.000000000000000000, 0.000000000000000000, -1.000000000000000000 ) ) ;
#2093 = FACE_OUTER_BOUND ( 'NONE', #8454, .T. ) ;
#2095 = ORIENTED_EDGE ( 'NONE', *, *, #3370, .F. ) ;
#2094 = AXIS2_PLACEMENT_3D ( 'NONE', #4822, #8719, #14516 ) ;
#2096 = CARTESIAN_POINT ( 'NONE',  ( -5.666074146197985328, 1.978051345703193187, 16.99995067926685977 ) ) ;
#2097 =( REPRESENTATION_RELATIONSHIP ('NONE','NONE', #11191, #11283 ) REPRESENTATION_RELATIONSHIP_WITH_TRANSFORMATION ( #971 )SHAPE_REPRESENTATION_RELATIONSHIP( ) );
#2098 = EDGE_CURVE ( 'NONE', #14280, #471, #13746, .T. ) ;
#2099 = CARTESIAN_POINT ( 'NONE',  ( -4.286401442266628337, -4.198423832313095794, 17.99999999999998934 ) ) ;
#2100 = CARTESIAN_POINT ( 'NONE',  ( -4.070051655338168040, 4.744673454622424735, 12.37367328635990660 ) ) ;
#2101 = CARTESIAN_POINT ( 'NONE',  ( -1.767766952966369098, 1.767766952966369098, 0.000000000000000000 ) ) ;
#2102 = CARTESIAN_POINT ( 'NONE',  ( -3.567258970016065955, -5.133675764669609620, 25.50008219321555458 ) ) ;
#2103 = CARTESIAN_POINT ( 'NONE',  ( 2.817313151351187983, -5.579000502529432026, 5.000000000000004441 ) ) ;
#2104 = CARTESIAN_POINT ( 'NONE',  ( 1.767766952966369320, 186.3999999978150584, 5.232233047033630235 ) ) ;
#2105 = EDGE_CURVE ( 'NONE', #6711, #2813, #8603, .T. ) ;
#2106 = CARTESIAN_POINT ( 'NONE',  ( 1.237590631448066469, 228.1696616696178808, 9.916980740552745033 ) ) ;
#2107 = CARTESIAN_POINT ( 'NONE',  ( -6.105925084677658710, -1.337450587213287356, 18.79933148907576523 ) ) ;
#2108 = DIRECTION ( 'NONE',  ( 0.000000000000000000, 1.000000000000000000, 0.000000000000000000 ) ) ;
#2109 = ADVANCED_FACE ( 'NONE', ( #11358 ), #1648, .F. ) ;
#2110 = LINE ( 'NONE', #13086, #8853 ) ;
#2111 = CARTESIAN_POINT ( 'NONE',  ( -1.035533905932737975, 188.2500000000000000, 4.500000000000000888 ) ) ;
#2112 = CARTESIAN_POINT ( 'NONE',  ( -4.435347140101218777, 4.403429997944323659, 24.49999999999999289 ) ) ;
#2114 = ORIENTED_EDGE ( 'NONE', *, *, #11739, .F. ) ;
#2113 = CARTESIAN_POINT ( 'NONE',  ( 5.131373506000437068, 7.062729720844210135, 24.49999999999999289 ) ) ;
#2115 = CARTESIAN_POINT ( 'NONE',  ( -6.142844459177225325, 1.156093792145259203, 18.61560192892921251 ) ) ;
#2116 =( REPRESENTATION_RELATIONSHIP ('NONE','NONE', #11191, #3660 ) REPRESENTATION_RELATIONSHIP_WITH_TRANSFORMATION ( #10762 )SHAPE_REPRESENTATION_RELATIONSHIP( ) );
#2117 = DIRECTION ( 'NONE',  ( 0.000000000000000000, 0.000000000000000000, 1.000000000000000000 ) ) ;
#2118 = LINE ( 'NONE', #9924, #11741 ) ;
#2119 = CARTESIAN_POINT ( 'NONE',  ( 6.143020266951002561, 1.155160780047578495, 25.11441947245484485 ) ) ;
#2120 = CARTESIAN_POINT ( 'NONE',  ( 1.035533905932737975, 185.6800000002185129, 4.500000000000000888 ) ) ;
#2121 = DIRECTION ( 'NONE',  ( -0.5877852522924685852, -0.8090169943749507819, 0.000000000000000000 ) ) ;
#2122 = CARTESIAN_POINT ( 'NONE',  ( 1.454231928715901123, 227.8150477629479269, 5.705238247175231869 ) ) ;
#2123 = CARTESIAN_POINT ( 'NONE',  ( 5.858736126997138527, 2.179962889277050841, 10.52640428276697726 ) ) ;
#2124 = CARTESIAN_POINT ( 'NONE',  ( -5.859221468178994918, 2.178708437343097160, 4.025914576658297328 ) ) ;
#2125 = DIRECTION ( 'NONE',  ( -1.000000000000000000, 0.000000000000000000, 0.000000000000000000 ) ) ;
#2126 = ORIENTED_EDGE ( 'NONE', *, *, #14143, .T. ) ;
#2127 = CARTESIAN_POINT ( 'NONE',  ( 0.8561741729129461742, 185.6999999989075434, 9.066987300000000971 ) ) ;
#2128 = CARTESIAN_POINT ( 'NONE',  ( 2.848727059636023018, 5.281416301279862502, 30.38557478428061742 ) ) ;
#2129 = ORIENTED_EDGE ( 'NONE', *, *, #7561, .T. ) ;
#2130 = ADVANCED_FACE ( 'NONE', ( #458 ), #12315, .F. ) ;
#2131 = CYLINDRICAL_SURFACE ( 'NONE', #13944, 1.000000000000000666 ) ;
#2132 = CARTESIAN_POINT ( 'NONE',  ( -4.196038884587202311, 4.289036423669238651, 31.50389795015983552 ) ) ;
#2133 = CARTESIAN_POINT ( 'NONE',  ( 2.817313151350985923, 5.579000502529535055, 17.86939309276500154 ) ) ;
#2134 = CARTESIAN_POINT ( 'NONE',  ( -2.066987300000000971, 187.7999999989075093, 6.143825827087054492 ) ) ;
#2135 = DIRECTION ( 'NONE',  ( -0.4999999999999998890, 0.8660254037844387076, 0.000000000000000000 ) ) ;
#2136 = CARTESIAN_POINT ( 'NONE',  ( -1.530808498934191571E-16, 2.500000000000000000, -1.599999997815050312 ) ) ;
#2137 = CARTESIAN_POINT ( 'NONE',  ( -5.000000000000000000, 0.000000000000000000, 2.000000000000001776 ) ) ;
#2138 = CARTESIAN_POINT ( 'NONE',  ( 5.999999999999999112, 187.9952603975225429, 3.440894205938198613 ) ) ;
#2139 = CARTESIAN_POINT ( 'NONE',  ( -1.767766952966368432, -1.767766952966369320, 1.000000000000000000 ) ) ;
#2140 = CARTESIAN_POINT ( 'NONE',  ( -5.317509234263866347, -2.779225709351170526, 17.86938304467859595 ) ) ;
#2141 = CARTESIAN_POINT ( 'NONE',  ( -0.1306171417087258479, -6.000000000000002665, 16.99999999999998224 ) ) ;
#2142 = VECTOR ( 'NONE', #101, 1000.000000000000000 ) ;
#2143 = ORIENTED_EDGE ( 'NONE', *, *, #2200, .F. ) ;
#2144 = ORIENTED_EDGE ( 'NONE', *, *, #12545, .F. ) ;
#2145 = ORIENTED_EDGE ( 'NONE', *, *, #494, .T. ) ;
#2146 = LINE ( 'NONE', #5085, #1906 ) ;
#2147 = DIRECTION ( 'NONE',  ( 0.000000000000000000, 0.000000000000000000, 1.000000000000000000 ) ) ;
#2148 = ORIENTED_EDGE ( 'NONE', *, *, #9837, .F. ) ;
#2149 = EDGE_CURVE ( 'NONE', #12720, #2410, #13507, .T. ) ;
#2150 = CARTESIAN_POINT ( 'NONE',  ( 3.796994071234844259E-16, -2.066987299999999639, 1.450000001092474733 ) ) ;
#2151 = CARTESIAN_POINT ( 'NONE',  ( -0.2622916576874523287, 5.995491482261837035, 25.47384942646813499 ) ) ;
#2152 = AXIS2_PLACEMENT_3D ( 'NONE', #15148, #11554, #12744 ) ;
#2153 = CARTESIAN_POINT ( 'NONE',  ( -4.416837305303439543, -4.422286678979068242, 4.738097869159890507 ) ) ;
#2154 = CARTESIAN_POINT ( 'NONE',  ( -1.461580736456472795, 184.7499999989074979, 5.538419263543527649 ) ) ;
#2155 = CARTESIAN_POINT ( 'NONE',  ( -1.035533905932737753, 2.500000000000000444, -0.04300000002184962283 ) ) ;
#2156 = CARTESIAN_POINT ( 'NONE',  ( -4.322356511625772058, 7.650514973136511188, 5.000000000000004441 ) ) ;
#2157 = CONTEXT_DEPENDENT_SHAPE_REPRESENTATION ( #6994, #672 ) ;
#2158 = CARTESIAN_POINT ( 'NONE',  ( 0.8561741729129451750, 2.066987299999999639, 1.000000001092474555 ) ) ;
#2159 = CARTESIAN_POINT ( 'NONE',  ( 2.840966774240303305, -5.567223638426833432, 4.738097869159889619 ) ) ;
#2160 = CARTESIAN_POINT ( 'NONE',  ( 2.961265621965179395, 227.4473031124620377, 7.792030372366526514 ) ) ;
#2161 = CARTESIAN_POINT ( 'NONE',  ( 1.035533905932737531, 2.500000000000000444, 0.7500000021849496656 ) ) ;
#2162 = ORIENTED_EDGE ( 'NONE', *, *, #6351, .F. ) ;
#2163 = CARTESIAN_POINT ( 'NONE',  ( -1.035533905932739529, 186.0499999978150356, 9.500000000000000000 ) ) ;
#2164 = VECTOR ( 'NONE', #6272, 1000.000000000000000 ) ;
#2165 = VERTEX_POINT ( 'NONE', #11281 ) ;
#2166 = ORIENTED_EDGE ( 'NONE', *, *, #7266, .T. ) ;
#2167 = CARTESIAN_POINT ( 'NONE',  ( -5.558508435838136919, 2.857531096719036601, 24.63060690723497359 ) ) ;
#2168 = EDGE_CURVE ( 'NONE', #1512, #7314, #4089, .T. ) ;
#2169 = CARTESIAN_POINT ( 'NONE',  ( -2.841041022017486650, -5.567186575787210323, 24.23774718278286500 ) ) ;
#2170 = CARTESIAN_POINT ( 'NONE',  ( -5.454892180317694184E-16, 185.4000000000000057, 9.500000000000001776 ) ) ;
#2171 = ORIENTED_EDGE ( 'NONE', *, *, #6889, .T. ) ;
#2172 = FACE_OUTER_BOUND ( 'NONE', #5920, .T. ) ;
#2173 = CARTESIAN_POINT ( 'NONE',  ( -0.1323408341374885389, -6.250000000000001776, 6.000000000000007105 ) ) ;
#2174 = FACE_BOUND ( 'NONE', #7752, .T. ) ;
#2175 = CARTESIAN_POINT ( 'NONE',  ( -3.567258970016013997, -5.133675764669648700, 19.00008219321555103 ) ) ;
#2176 = CARTESIAN_POINT ( 'NONE',  ( 0.7993282387952456158, -5.947240459526492273, 18.61484358216956636 ) ) ;
#2177 = FACE_OUTER_BOUND ( 'NONE', #6106, .T. ) ;
#2178 = CARTESIAN_POINT ( 'NONE',  ( 0.03680535197730239877, 0.4000000000000097367, -2.530258816757608997 ) ) ;
#2179 = CARTESIAN_POINT ( 'NONE',  ( 2.500000000000000444, 188.0500000000000114, 5.964466094067262247 ) ) ;
#2180 = ADVANCED_FACE ( 'NONE', ( #2774 ), #3877, .T. ) ;
#2181 = CARTESIAN_POINT ( 'NONE',  ( -1.212431555520800508, 228.7775460029053534, 8.484988061474600940 ) ) ;
#2182 = CARTESIAN_POINT ( 'NONE',  ( -6.081464507797595509, -1.446657058464349666, 18.87380055247394850 ) ) ;
#2183 = CARTESIAN_POINT ( 'NONE',  ( -0.1126307680551840440, 188.9999999999637623, 4.495745018146146244 ) ) ;
#2184 = ORIENTED_EDGE ( 'NONE', *, *, #5963, .T. ) ;
#2185 = CARTESIAN_POINT ( 'NONE',  ( -2.782769401326203429, 5.315896561274835896, 4.495710796379801977 ) ) ;
#2186 = CIRCLE ( 'NONE', #9077, 12.50000000000000355 ) ;
#2187 = CARTESIAN_POINT ( 'NONE',  ( -0.6144377077729259451, -5.969178481556073557, 10.70033966857734775 ) ) ;
#2189 = ORIENTED_EDGE ( 'NONE', *, *, #14283, .T. ) ;
#2188 = CARTESIAN_POINT ( 'NONE',  ( -0.5031281619705731956, -5.980084330432684503, 23.62602272744524967 ) ) ;
#2190 = CYLINDRICAL_SURFACE ( 'NONE', #988, 1.000000000000000888 ) ;
#2191 = DIRECTION ( 'NONE',  ( -0.9510565162951544194, 0.3090169943749447312, 0.000000000000000000 ) ) ;
#2192 = ORIENTED_EDGE ( 'NONE', *, *, #3958, .F. ) ;
#2193 = CARTESIAN_POINT ( 'NONE',  ( -5.621278735166179708, 2.101423246382604582, 23.52591947216898305 ) ) ;
#2194 = CARTESIAN_POINT ( 'NONE',  ( -2.175328470913686196, 226.6252516911083603, 5.371125302583743988 ) ) ;
#2195 = EDGE_CURVE ( 'NONE', #9577, #3564, #5089, .T. ) ;
#2196 =( NAMED_UNIT ( * ) SI_UNIT ( $, .STERADIAN. ) SOLID_ANGLE_UNIT ( ) );
#2197 = CARTESIAN_POINT ( 'NONE',  ( 6.176542424588136626, 0.9554180641284277797, 24.49999999999999289 ) ) ;
#2198 = CARTESIAN_POINT ( 'NONE',  ( -5.895349312889930360E-16, 186.1300000002185016, 9.500000000000001776 ) ) ;
#2199 = DIRECTION ( 'NONE',  ( -0.000000000000000000, 1.000000000000000000, -0.000000000000000000 ) ) ;
#2200 = EDGE_CURVE ( 'NONE', #2929, #7504, #330, .T. ) ;
#2201 = CIRCLE ( 'NONE', #15686, 1.499999999999999556 ) ;
#2202 = CARTESIAN_POINT ( 'NONE',  ( -1.618809023786734747, 227.8806835185142461, 5.894798052868548410 ) ) ;
#2203 = FACE_BOUND ( 'NONE', #15210, .T. ) ;
#2204 = CARTESIAN_POINT ( 'NONE',  ( -1.265664690411614835E-16, 2.066987299999999639, -0.3499999989075254225 ) ) ;
#2205 = CARTESIAN_POINT ( 'NONE',  ( -4.143041610105294481, -4.340967609747044875, 30.38602261056917442 ) ) ;
#2206 = EDGE_CURVE ( 'NONE', #15154, #14884, #5871, .T. ) ;
#2207 = EDGE_LOOP ( 'NONE', ( #744, #15528 ) ) ;
#2208 = CARTESIAN_POINT ( 'NONE',  ( -1.965116437629976787E-16, 189.2499999989075263, 4.933012699999999029 ) ) ;
#2209 = FACE_OUTER_BOUND ( 'NONE', #12234, .T. ) ;
#2210 = ORIENTED_EDGE ( 'NONE', *, *, #14325, .T. ) ;
#2211 = DIRECTION ( 'NONE',  ( 0.000000000000000000, 0.000000000000000000, 1.000000000000000000 ) ) ;
#2212 = CARTESIAN_POINT ( 'NONE',  ( 5.558508435838189321, 2.857531096718932240, 5.000000000000004441 ) ) ;
#2213 = DIRECTION ( 'NONE',  ( -0.5877852522924685852, -0.8090169943749507819, 0.000000000000000000 ) ) ;
#2214 = CARTESIAN_POINT ( 'NONE',  ( 9.750000000000003553, 182.0000000000000000, 1.020968533498575461E-13 ) ) ;
#2215 = CARTESIAN_POINT ( 'NONE',  ( -0.8561741729129457301, 186.0999999989074922, 4.933012699999999029 ) ) ;
#2216 = CARTESIAN_POINT ( 'NONE',  ( 4.005998022990015173, -4.467726698309212097, 30.20068193741824913 ) ) ;
#2217 = CARTESIAN_POINT ( 'NONE',  ( 1.767766952966369320, -1.767766952966368654, 0.5000000021849496656 ) ) ;
#2218 = CARTESIAN_POINT ( 'NONE',  ( 3.736691294293456700, -4.695920479336350262, 10.52641404563304839 ) ) ;
#2219 = CARTESIAN_POINT ( 'NONE',  ( 0.000000000000000000, 187.2933328889893687, 9.583808270834989429 ) ) ;
#2221 = CARTESIAN_POINT ( 'NONE',  ( 1.035533905932739085, -2.500000000000000000, 1.149999999999999689 ) ) ;
#2220 = AXIS2_PLACEMENT_3D ( 'NONE', #9988, #11329, #14915 ) ;
#2222 = CARTESIAN_POINT ( 'NONE',  ( 5.782895619916144980, 1.604017620858124271, 4.025919472168997260 ) ) ;
#2223 = CARTESIAN_POINT ( 'NONE',  ( -0.6156307853268060404, -5.969051238897268519, 18.79870573410680379 ) ) ;
#2224 = ORIENTED_EDGE ( 'NONE', *, *, #5208, .F. ) ;
#2225 = B_SPLINE_CURVE_WITH_KNOTS ( 'NONE', 3,
 ( #8320, #7208, #9589, #3614, #13159, #11966, #10780, #4740, #8569, #12048, #15638, #3537, #15722, #1147, #9677, #115, #8408, #14515 ),
 .UNSPECIFIED., .F., .F.,
 ( 4, 2, 2, 2, 2, 2, 2, 2, 4 ),
 ( 0.000000000000000000, 0.0003914898357794963026, 0.0007829796715589926051, 0.001174469507338488962, 0.001565959343117985210, 0.001957449178897481459, 0.002348939014676977924, 0.002740428850456473955, 0.003131918686235970421 ),
 .UNSPECIFIED. ) ;
#2226 = ORIENTED_EDGE ( 'NONE', *, *, #8279, .F. ) ;
#2227 = EDGE_LOOP ( 'NONE', ( #15670, #11895 ) ) ;
#2228 = CARTESIAN_POINT ( 'NONE',  ( 4.435347140100996732, 4.403429997944549257, 30.86765874365831408 ) ) ;
#2229 = CARTESIAN_POINT ( 'NONE',  ( 1.583819872848719834, 227.8634474321731034, 5.845019252434271451 ) ) ;
#2230 = ORIENTED_EDGE ( 'NONE', *, *, #14566, .F. ) ;
#2231 = ADVANCED_FACE ( 'NONE', ( #10696 ), #987, .T. ) ;
#2232 = CARTESIAN_POINT ( 'NONE',  ( 2.500000000000000444, 1.035533905932737975, -2.549999997815051156 ) ) ;
#2233 = CARTESIAN_POINT ( 'NONE',  ( -0.9999502950800045475, 5.916088184763918179, 24.63108149190010820 ) ) ;
#2234 = DIRECTION ( 'NONE',  ( -0.000000000000000000, 1.000000000000000000, -0.000000000000000000 ) ) ;
#2235 = CARTESIAN_POINT ( 'NONE',  ( -2.066987300000000527, 188.0499999989075093, 7.000000000000000000 ) ) ;
#2236 = CARTESIAN_POINT ( 'NONE',  ( -2.500000000000000000, 0.000000000000000000, 0.1069999999781503230 ) ) ;
#2237 = DIRECTION ( 'NONE',  ( -1.000000000000000000, 3.326610055774637112E-18, 1.062480551894331163E-17 ) ) ;
#2238 = CONTEXT_DEPENDENT_SHAPE_REPRESENTATION ( #9448, #8056 ) ;
#2239 = CARTESIAN_POINT ( 'NONE',  ( 2.066987299999999639, 2.531329380823229670E-16, -0.7499999989075251117 ) ) ;
#2240 = EDGE_CURVE ( 'NONE', #10282, #13993, #5485, .T. ) ;
#2241 = CARTESIAN_POINT ( 'NONE',  ( 2.840966774240286430, -5.567223638426841426, 30.73809786915987274 ) ) ;
#2242 = CARTESIAN_POINT ( 'NONE',  ( 2.856278104602718138, 227.5851434513726019, 8.197675965640897289 ) ) ;
#2243 = LINE ( 'NONE', #5997, #8257 ) ;
#2244 = EDGE_LOOP ( 'NONE', ( #13848, #357 ) ) ;
#2245 = AXIS2_PLACEMENT_3D ( 'NONE', #11936, #1042, #3422 ) ;
#2246 = ORIENTED_EDGE ( 'NONE', *, *, #10297, .T. ) ;
#2247 = DIRECTION ( 'NONE',  ( 6.123233995736766036E-17, -1.000000000000000000, -0.000000000000000000 ) ) ;
#2248 = VERTEX_POINT ( 'NONE', #2334 ) ;
#2250 = ORIENTED_EDGE ( 'NONE', *, *, #4656, .T. ) ;
#2249 = B_SPLINE_CURVE_WITH_KNOTS ( 'NONE', 3,
 ( #12899, #2313, #2151, #8217, #5599, #8381, #11631, #731, #2233, #9406, #14242, #13053, #7026, #11854, #15613, #5831, #2000, #4633 ),
 .UNSPECIFIED., .F., .F.,
 ( 4, 2, 2, 2, 2, 2, 2, 2, 4 ),
 ( 0.000000000000000000, 0.0003914904498596244128, 0.0007829808997192488256, 0.001174471349578873293, 0.001565961799438497651, 0.001957452249298122227, 0.002348942699157746585, 0.002740433149017370944, 0.003131923598876995302 ),
 .UNSPECIFIED. ) ;
#2251 = CARTESIAN_POINT ( 'NONE',  ( 0.8730628416137486969, 6.188929913094962210, 30.49504929893118899 ) ) ;
#2252 = CARTESIAN_POINT ( 'NONE',  ( -2.931156713028560734, -5.520271803279174883, 23.99563030319847812 ) ) ;
#2253 = CARTESIAN_POINT ( 'NONE',  ( -1.035533905932739529, 185.3499999999999943, 9.500000000000000000 ) ) ;
#2254 = ORIENTED_EDGE ( 'NONE', *, *, #7655, .F. ) ;
#2255 = DIRECTION ( 'NONE',  ( 0.000000000000000000, 0.000000000000000000, -1.000000000000000000 ) ) ;
#2256 = CARTESIAN_POINT ( 'NONE',  ( 5.317509234264033324, -2.779225709350852114, 17.99999999999998934 ) ) ;
#2257 = DIRECTION ( 'NONE',  ( 0.000000000000000000, 0.000000000000000000, -1.000000000000000000 ) ) ;
#2258 = CARTESIAN_POINT ( 'NONE',  ( -4.435347140101121965, 4.403429997944421359, 11.49999999999998224 ) ) ;
#2259 = CARTESIAN_POINT ( 'NONE',  ( -6.081509788407695183, -1.446521464462901196, 23.62618035954929141 ) ) ;
#2260 = CARTESIAN_POINT ( 'NONE',  ( -2.817313151351291012, -5.579000502529381400, 24.63234125634167526 ) ) ;
#2261 = SURFACE_SIDE_STYLE ('',( #11731 ) ) ;
#2262 = CARTESIAN_POINT ( 'NONE',  ( -2.500000000000000444, 186.6499999978150299, 5.964466094067261359 ) ) ;
#2263 = CARTESIAN_POINT ( 'NONE',  ( 0.1954887924997270876, 228.2535971796124556, 10.16375797564445804 ) ) ;
#2264 = CARTESIAN_POINT ( 'NONE',  ( 3.011899281037421883, 5.190111395030274188, 31.80022217383877958 ) ) ;
#2265 = CARTESIAN_POINT ( 'NONE',  ( -1.815566070620405315, 190.0296528384676549, 4.819757843237718831 ) ) ;
#2266 = ORIENTED_EDGE ( 'NONE', *, *, #1610, .F. ) ;
#2267 = DIRECTION ( 'NONE',  ( 0.5877852522924802425, -0.8090169943749422332, 0.000000000000000000 ) ) ;
#2268 = AXIS2_PLACEMENT_3D ( 'NONE', #14846, #11337, #6504 ) ;
#2269 = CARTESIAN_POINT ( 'NONE',  ( 4.286401442266438266, 4.198423832313292081, 17.86763921416087797 ) ) ;
#2270 = B_SPLINE_CURVE_WITH_KNOTS ( 'NONE', 3,
 ( #4615, #4536, #15516, #7084, #11691, #790, #13996, #1901, #9468, #13113, #11921, #3252, #3332, #5657, #945, #10503, #15359, #5581 ),
 .UNSPECIFIED., .F., .F.,
 ( 4, 2, 2, 2, 2, 2, 2, 2, 4 ),
 ( 0.000000000000000000, 0.0003914898357794948389, 0.0007829796715589896778, 0.001174469507338484625, 0.001565959343117979356, 0.001957449178897474086, 0.002348939014676969250, 0.002740428850456463981, 0.003131918686235958711 ),
 .UNSPECIFIED. ) ;
#2272 = ORIENTED_EDGE ( 'NONE', *, *, #15433, .F. ) ;
#2271 = FACE_OUTER_BOUND ( 'NONE', #6770, .T. ) ;
#2273 = CARTESIAN_POINT ( 'NONE',  ( 0.01099607048649087204, -0.3999999999999993006, 2.497144250189434533 ) ) ;
#2274 = CARTESIAN_POINT ( 'NONE',  ( 2.363901779514900880, 226.6922819415928245, 5.568617383738656557 ) ) ;
#2275 = ORIENTED_EDGE ( 'NONE', *, *, #7022, .T. ) ;
#2276 = CARTESIAN_POINT ( 'NONE',  ( -4.006441409774651241, -4.467329318258288495, 5.798882422479411325 ) ) ;
#2277 = CARTESIAN_POINT ( 'NONE',  ( 1.461580736456473018, -1.461580736456472573, 0.9500000010924747329 ) ) ;
#2278 = CARTESIAN_POINT ( 'NONE',  ( -1.485687618429907486, 226.4511214500596168, 4.857910484922783212 ) ) ;
#2279 = FILL_AREA_STYLE ('',( #13180 ) ) ;
#2280 = CARTESIAN_POINT ( 'NONE',  ( -0.6156133477426608547, -6.220296490279944024, 31.79872387345512053 ) ) ;
#2281 = CARTESIAN_POINT ( 'NONE',  ( 1.767766952966368432, 187.0300000002185072, 8.767766952966368876 ) ) ;
#2282 = CARTESIAN_POINT ( 'NONE',  ( -2.997451966578419835, 5.485105005466003547, 5.615177803758428787 ) ) ;
#2283 = CARTESIAN_POINT ( 'NONE',  ( -1.361823383409473953, 227.7851450847494448, 5.618877607002349173 ) ) ;
#2284 = CARTESIAN_POINT ( 'NONE',  ( 6.105747081304174095, 1.338335777572260854, 10.69973484982323342 ) ) ;
#2285 = CARTESIAN_POINT ( 'NONE',  ( 1.461580736456473018, -1.461580736456472573, 0.9500000010924747329 ) ) ;
#2286 = ORIENTED_EDGE ( 'NONE', *, *, #7412, .T. ) ;
#2287 = CARTESIAN_POINT ( 'NONE',  ( 5.940390500375388072, 6.474944468551740329, 24.49999999999999289 ) ) ;
#2288 = CARTESIAN_POINT ( 'NONE',  ( 1.461580736456472795, 185.7499999989074979, 8.461580736456474128 ) ) ;
#2289 = CARTESIAN_POINT ( 'NONE',  ( 5.915699123067185816, 1.003533581835384769, 23.99610204984015382 ) ) ;
#2290 = EDGE_CURVE ( 'NONE', #6278, #6786, #11548, .T. ) ;
#2291 = ORIENTED_EDGE ( 'NONE', *, *, #3366, .F. ) ;
#2292 = EDGE_CURVE ( 'NONE', #7333, #703, #8327, .T. ) ;
#2293 = CARTESIAN_POINT ( 'NONE',  ( -4.196038884587270701, -4.289036423669171150, 23.99610204984015738 ) ) ;
#2294 = CARTESIAN_POINT ( 'NONE',  ( 0.2619041840696964552, -6.245686665308495478, 23.52605849433794916 ) ) ;
#2295 = DIRECTION ( 'NONE',  ( 6.123233995736766036E-17, -1.000000000000000000, -0.000000000000000000 ) ) ;
#2296 = CARTESIAN_POINT ( 'NONE',  ( -5.131373506000769247, 7.062729720843990755, 11.49999999999998224 ) ) ;
#2297 = CARTESIAN_POINT ( 'NONE',  ( -1.461580736456473906, 187.9499999989075150, 8.461580736456474128 ) ) ;
#2298 = CARTESIAN_POINT ( 'NONE',  ( 4.286401442266496886, -4.198423832313229020, 17.99999999999998934 ) ) ;
#2299 = CARTESIAN_POINT ( 'NONE',  ( 1.767766952966369320, -1.767766952966368654, 1.300000002184949821 ) ) ;
#2300 = CARTESIAN_POINT ( 'NONE',  ( -5.769755079862298963, -2.405651898699021629, 4.126941084456994702 ) ) ;
#2301 = CARTESIAN_POINT ( 'NONE',  ( 5.375886393124385876, -2.665038680141283756, 31.50439760644212939 ) ) ;
#2302 = CARTESIAN_POINT ( 'NONE',  ( -1.768703179866833342, 189.0000639513403939, 5.233169770031948609 ) ) ;
#2303 = CARTESIAN_POINT ( 'NONE',  ( -6.142908455506947085, 1.155755562476039833, 10.88482219624155967 ) ) ;
#2304 = CYLINDRICAL_SURFACE ( 'NONE', #13300, 1.500000000000000000 ) ;
#2305 = ORIENTED_EDGE ( 'NONE', *, *, #2400, .F. ) ;
#2306 = VERTEX_POINT ( 'NONE', #12706 ) ;
#2307 = EDGE_CURVE ( 'NONE', #10183, #7094, #8724, .T. ) ;
#2308 = ORIENTED_EDGE ( 'NONE', *, *, #15367, .T. ) ;
#2309 = CARTESIAN_POINT ( 'NONE',  ( 1.938829455441115623, 228.0900040983942745, 6.499327826426426924 ) ) ;
#2310 = EDGE_LOOP ( 'NONE', ( #1236, #473 ) ) ;
#2311 = PRODUCT ( 'strain limiting mesh layer', 'strain limiting mesh layer', '', ( #5135 ) ) ;
#2312 = CARTESIAN_POINT ( 'NONE',  ( 1.035533905932739085, -2.500000000000000000, -2.749999997815050445 ) ) ;
#2313 = CARTESIAN_POINT ( 'NONE',  ( -0.1323933160973585210, 6.000000000000004441, 25.49999999999999289 ) ) ;
#2314 = CARTESIAN_POINT ( 'NONE',  ( 6.176542424588110869, 0.9554180641286114106, 31.13060690723498425 ) ) ;
#2315 = CARTESIAN_POINT ( 'NONE',  ( -2.066987300000000083, 187.1999999989075434, 6.143825827087054492 ) ) ;
#2316 = CARTESIAN_POINT ( 'NONE',  ( -1.530808498934191571E-16, 2.500000000000000000, -0.09300000002184975745 ) ) ;
#2317 = FACE_OUTER_BOUND ( 'NONE', #1081, .T. ) ;
#2318 = CARTESIAN_POINT ( 'NONE',  ( -1.461580736456472351, -1.461580736456473018, 1.550000001092474822 ) ) ;
#2319 = DIRECTION ( 'NONE',  ( -6.123233995736766036E-17, 1.000000000000000000, 0.000000000000000000 ) ) ;
#2320 = CARTESIAN_POINT ( 'NONE',  ( -0.9181233697252281223, 226.3712865412501003, 4.622592831843514993 ) ) ;
#2321 = CARTESIAN_POINT ( 'NONE',  ( 2.500000000000000444, 187.2000000000000171, 7.000000000000000000 ) ) ;
#2322 = ORIENTED_EDGE ( 'NONE', *, *, #13868, .T. ) ;
#2323 = AXIS2_PLACEMENT_3D ( 'NONE', #6472, #7570, #1435 ) ;
#2324 = ORIENTED_EDGE ( 'NONE', *, *, #11630, .T. ) ;
#2325 = CARTESIAN_POINT ( 'NONE',  ( 0.09128442572522987852, 0.000000000000000000, 0.000000000000000000 ) ) ;
#2326 = VERTEX_POINT ( 'NONE', #611 ) ;
#2327 = ORIENTED_EDGE ( 'NONE', *, *, #5021, .F. ) ;
#2328 = CARTESIAN_POINT ( 'NONE',  ( 0.9737725088282426222, 6.173885267451817427, 30.73735758726564882 ) ) ;
#2329 = CARTESIAN_POINT ( 'NONE',  ( -3.567624405365383833, -5.133384272590680197, 23.50004921015705150 ) ) ;
#2330 = CARTESIAN_POINT ( 'NONE',  ( 0.8736772044959983941, -6.188841968496061163, 4.496115732928122277 ) ) ;
#2331 = ADVANCED_FACE ( 'NONE', ( #10328 ), #9674, .F. ) ;
#2332 = CARTESIAN_POINT ( 'NONE',  ( -5.570722351696249852, -2.834100162821999280, 31.26190213084010239 ) ) ;
#2333 = UNCERTAINTY_MEASURE_WITH_UNIT (LENGTH_MEASURE( 1.000000000000000082E-05 ), #8736, 'distance_accuracy_value', 'NONE');
#2334 = CARTESIAN_POINT ( 'NONE',  ( 2.031800923283433283E-13, -6.000000000000000888, 23.49999999999999289 ) ) ;
#2335 = PRODUCT_DEFINITION ( 'UNKNOWN', '', #9596, #7853 ) ;
#2336 = FACE_BOUND ( 'NONE', #14082, .T. ) ;
#2337 = VECTOR ( 'NONE', #10079, 1000.000000000000000 ) ;
#2339 = FACE_OUTER_BOUND ( 'NONE', #9666, .T. ) ;
#2338 = B_SPLINE_CURVE_WITH_KNOTS ( 'NONE', 3,
 ( #10075, #207, #8893, #11262, #2834, #11104, #5310, #11339, #7681, #362, #12530, #6266, #3934, #15084, #9049, #436, #5386, #2910 ),
 .UNSPECIFIED., .F., .F.,
 ( 4, 2, 2, 2, 2, 2, 2, 2, 4 ),
 ( 0.003131486019301959502, 0.003522824630466669243, 0.003914163241631378985, 0.004305501852796088727, 0.004696840463960799336, 0.005088179075125509945, 0.005479517686290219687, 0.005870856297454930296, 0.006262194908619640905 ),
 .UNSPECIFIED. ) ;
#2340 = EDGE_CURVE ( 'NONE', #13429, #8130, #2827, .T. ) ;
#2341 = CARTESIAN_POINT ( 'NONE',  ( -5.903061651806536858, -2.057626436184982754, 23.50008258189710020 ) ) ;
#2342 = DIRECTION ( 'NONE',  ( 1.251928832280965695E-16, 1.000000000000000000, 0.000000000000000000 ) ) ;
#2343 = DIRECTION ( 'NONE',  ( 0.000000000000000000, -1.000000000000000000, 0.000000000000000000 ) ) ;
#2344 = CARTESIAN_POINT ( 'NONE',  ( 1.767766952966368432, 186.9999999978150527, 8.767766952966368876 ) ) ;
#2345 = CARTESIAN_POINT ( 'NONE',  ( 2.976061188595913176, 227.1638826975962502, 6.957706536906315797 ) ) ;
#2346 = CARTESIAN_POINT ( 'NONE',  ( -6.176542424588083335, -0.9554180641287667308, 17.99999999999998934 ) ) ;
#2347 = CARTESIAN_POINT ( 'NONE',  ( 5.317509234263941842, 2.779225709351030638, 31.00000000000000000 ) ) ;
#2348 = VECTOR ( 'NONE', #3673, 1000.000000000000000 ) ;
#2349 = ORIENTED_EDGE ( 'NONE', *, *, #11851, .F. ) ;
#2350 = CARTESIAN_POINT ( 'NONE',  ( 5.317509234263963158, 2.779225709350988449, 11.49999999999998224 ) ) ;
#2351 = B_SPLINE_CURVE_WITH_KNOTS ( 'NONE', 3,
 ( #13311, #2167, #8483, #7040, #4571, #9667, #2412, #3605, #4733, #13236, #7279, #10691, #6964, #15551, #12115, #1217, #6087, #10929 ),
 .UNSPECIFIED., .F., .F.,
 ( 4, 2, 2, 2, 2, 2, 2, 2, 4 ),
 ( 0.003131486019301974680, 0.003522824630466682688, 0.003914163241631390261, 0.004305501852796098268, 0.004696840463960806275, 0.005088179075125514282, 0.005479517686290222289, 0.005870856297454930296, 0.006262194908619638303 ),
 .UNSPECIFIED. ) ;
#2352 = LINE ( 'NONE', #14611, #7682 ) ;
#2354 = ORIENTED_EDGE ( 'NONE', *, *, #11370, .T. ) ;
#2353 = CARTESIAN_POINT ( 'NONE',  ( 5.867109477881260027, 1.259218163100832566, 25.29888242247940866 ) ) ;
#2355 = CARTESIAN_POINT ( 'NONE',  ( 0.03964714319856429969, -0.3999999999999923617, 2.532520041490997187 ) ) ;
#2356 = CARTESIAN_POINT ( 'NONE',  ( 2.500000000000000000, 3.061616997868383141E-16, -0.1999999978150501789 ) ) ;
#2357 = ORIENTED_EDGE ( 'NONE', *, *, #8275, .T. ) ;
#2358 = CARTESIAN_POINT ( 'NONE',  ( 2.841163418881210490, 5.567120626448023302, 24.23763026556123279 ) ) ;
#2359 = CARTESIAN_POINT ( 'NONE',  ( -1.461580736456472351, -1.461580736456473018, -0.04999999890752505893 ) ) ;
#2360 = CARTESIAN_POINT ( 'NONE',  ( -2.773146674828778302, 226.9215239162201669, 6.243979701131443072 ) ) ;
#2361 = CARTESIAN_POINT ( 'NONE',  ( -5.725684683139623310, 2.507514573674738845, 12.29887838423337953 ) ) ;
#2362 = CARTESIAN_POINT ( 'NONE',  ( 2.500000000000000000, 188.7300000002184959, 7.000000000000000000 ) ) ;
#2363 = CARTESIAN_POINT ( 'NONE',  ( -2.940898392866930777E-15, 228.9118723800512498, 8.872930300147352511 ) ) ;
#2364 = CARTESIAN_POINT ( 'NONE',  ( -1.454198809819935878, 227.8150368499753995, 5.705206729889046535 ) ) ;
#2365 = CARTESIAN_POINT ( 'NONE',  ( 1.895314869936763680, 228.4599366835234093, 7.567714231851713436 ) ) ;
#2366 = CARTESIAN_POINT ( 'NONE',  ( -0.8561741729129458411, -2.066987299999999195, -0.7999999989075252671 ) ) ;
#2367 = CARTESIAN_POINT ( 'NONE',  ( -2.500000000000000000, 0.000000000000000000, 1.700000000000000178 ) ) ;
#2368 = ORIENTED_EDGE ( 'NONE', *, *, #6341, .T. ) ;
#2369 = CARTESIAN_POINT ( 'NONE',  ( -2.066987300000001415, 187.7999999989075093, 6.143825827087054492 ) ) ;
#2370 = CARTESIAN_POINT ( 'NONE',  ( -2.066987300000000971, 185.3999999989075604, 6.143825827087054492 ) ) ;
#2371 = CARTESIAN_POINT ( 'NONE',  ( -2.500000000000000000, 0.000000000000000000, 1.800000002184949821 ) ) ;
#2372 = ORIENTED_EDGE ( 'NONE', *, *, #6889, .F. ) ;
#2373 = AXIS2_PLACEMENT_3D ( 'NONE', #7244, #4937, #9866 ) ;
#2374 = DIRECTION ( 'NONE',  ( 0.000000000000000000, 1.000000000000000000, 0.000000000000000000 ) ) ;
#2375 = EDGE_CURVE ( 'NONE', #2588, #10768, #2052, .T. ) ;
#2376 = CARTESIAN_POINT ( 'NONE',  ( 0.000000000000000000, 0.000000000000000000, 0.000000000000000000 ) ) ;
#2377 = FACE_OUTER_BOUND ( 'NONE', #14707, .T. ) ;
#2378 = CARTESIAN_POINT ( 'NONE',  ( 0.7995524673975999974, 6.199337389817264565, 12.11453679452461429 ) ) ;
#2379 = CARTESIAN_POINT ( 'NONE',  ( 0.8561741729129461742, 186.4999999989074695, 9.066987300000000971 ) ) ;
#2380 = CARTESIAN_POINT ( 'NONE',  ( 4.267936573529138577, 4.217499624512312195, 18.26229037835932090 ) ) ;
#2381 = CARTESIAN_POINT ( 'NONE',  ( 2.500000000000000000, 3.061616997868383141E-16, 0.5000000000000000000 ) ) ;
#2382 = CARTESIAN_POINT ( 'NONE',  ( -0.7995298244854430747, -5.947211616899250153, 31.61456014619858124 ) ) ;
#2383 = CARTESIAN_POINT ( 'NONE',  ( 2.500000000000000444, 184.0499999999999829, 5.964466094067262247 ) ) ;
#2384 = CARTESIAN_POINT ( 'NONE',  ( -0.9999171162588356143, -6.169494774098570389, 17.86722320330672886 ) ) ;
#2385 = CARTESIAN_POINT ( 'NONE',  ( -6.021167129161070442, 1.680051667990249520, 10.52640428276697548 ) ) ;
#2386 = CARTESIAN_POINT ( 'NONE',  ( -5.866984344570854049, 1.259800266528525725, 30.20068193741825624 ) ) ;
#2387 = EDGE_CURVE ( 'NONE', #5765, #7968, #2736, .T. ) ;
#2388 = ORIENTED_EDGE ( 'NONE', *, *, #15476, .F. ) ;
#2389 = EDGE_LOOP ( 'NONE', ( #13309, #7223, #2539, #4850 ) ) ;
#2390 = ORIENTED_EDGE ( 'NONE', *, *, #771, .T. ) ;
#2391 = CYLINDRICAL_SURFACE ( 'NONE', #9882, 1.000000000000000888 ) ;
#2392 = ORIENTED_EDGE ( 'NONE', *, *, #11914, .F. ) ;
#2393 = CARTESIAN_POINT ( 'NONE',  ( -0.8561741729129455081, 2.066987299999999639, 1.900000001092474688 ) ) ;
#2394 = CARTESIAN_POINT ( 'NONE',  ( 7.347881242120658060E-16, 6.000000000000000888, 4.000000000000004441 ) ) ;
#2395 = CARTESIAN_POINT ( 'NONE',  ( -5.317509234263900098, -2.779225709351108797, 11.49999999999998224 ) ) ;
#2396 = CARTESIAN_POINT ( 'NONE',  ( 1.461580736456472351, 186.7499999989075263, 8.461580736456474128 ) ) ;
#2397 = CARTESIAN_POINT ( 'NONE',  ( -1.767766952966369098, 1.767766952966369098, 0.7999999999999999334 ) ) ;
#2398 = CIRCLE ( 'NONE', #5980, 5.000000000000000000 ) ;
#2399 = CARTESIAN_POINT ( 'NONE',  ( -5.842988226680579267, 1.369004370660639180, 31.87380682714711355 ) ) ;
#2400 = EDGE_CURVE ( 'NONE', #7812, #1570, #4917, .T. ) ;
#2401 = ITEM_DEFINED_TRANSFORMATION ( 'NONE', 'NONE', #12196,  #14201 ) ;
#2402 = CARTESIAN_POINT ( 'NONE',  ( -0.8561741729129458411, -2.066987299999999195, -1.799999998907525267 ) ) ;
#2403 = CARTESIAN_POINT ( 'NONE',  ( 3.883716939929148459, -4.898343590941119707, 4.026404282766995912 ) ) ;
#2404 = CARTESIAN_POINT ( 'NONE',  ( -1.238695443643032412, 228.1695118093442716, 9.916540120957755278 ) ) ;
#2405 = LINE ( 'NONE', #7004, #15628 ) ;
#2406 = VERTEX_POINT ( 'NONE', #33 ) ;
#2407 = ORIENTED_EDGE ( 'NONE', *, *, #15632, .T. ) ;
#2408 = ADVANCED_FACE ( 'NONE', ( #8566 ), #1536, .F. ) ;
#2409 = CARTESIAN_POINT ( 'NONE',  ( 1.767766952966368654, 186.1999999978150697, 8.767766952966368876 ) ) ;
#2410 = VERTEX_POINT ( 'NONE', #7285 ) ;
#2411 = ORIENTED_EDGE ( 'NONE', *, *, #8456, .T. ) ;
#2412 = CARTESIAN_POINT ( 'NONE',  ( -5.769755079862251890, 2.405651898699137092, 25.37305891554299819 ) ) ;
#2413 = CLOSED_SHELL ( 'NONE', ( #10324, #3176, #13081, #10084, #10515, #11545 ) ) ;
#2414 = CARTESIAN_POINT ( 'NONE',  ( 4.005998022989933460, -4.467726698309286704, 17.20068193741824558 ) ) ;
#2415 = DIRECTION ( 'NONE',  ( 0.000000000000000000, 0.000000000000000000, -1.000000000000000000 ) ) ;
#2416 = EDGE_CURVE ( 'NONE', #5984, #11745, #7358, .T. ) ;
#2417 = CARTESIAN_POINT ( 'NONE',  ( 2.848727059636059433, -5.281416301279842962, 12.11442521571937192 ) ) ;
#2418 = CARTESIAN_POINT ( 'NONE',  ( 2.840966774240121673, -5.567223638426926691, 24.23809786915986919 ) ) ;
#2419 = FACE_BOUND ( 'NONE', #9726, .T. ) ;
#2420 = CARTESIAN_POINT ( 'NONE',  ( -3.779082820360738282, 4.979770177899218275, 12.50004906876531230 ) ) ;
#2421 = CARTESIAN_POINT ( 'NONE',  ( 0.2622916576877915573, -5.995491482261821048, 18.97384942646813144 ) ) ;
#2422 = CARTESIAN_POINT ( 'NONE',  ( -1.361387964035781121E-13, 26.00000000000000355, 9.750000000000003553 ) ) ;
#2423 = CARTESIAN_POINT ( 'NONE',  ( -2.500000000000000444, 187.5499999978150356, 8.035533905932737753 ) ) ;
#2424 = CARTESIAN_POINT ( 'NONE',  ( 2.843216347914732101, 226.9801049014886587, 6.416521247196312672 ) ) ;
#2425 = AXIS2_PLACEMENT_3D ( 'NONE', #10542, #15483, #4496 ) ;
#2426 = CARTESIAN_POINT ( 'NONE',  ( 5.726049995854516794, -2.506679546901767974, 17.20045537531157365 ) ) ;
#2427 = EDGE_CURVE ( 'NONE', #13484, #14260, #6091, .T. ) ;
#2428 = CARTESIAN_POINT ( 'NONE',  ( -2.276077516478379525, 188.9999999996472866, 5.950350810759988285 ) ) ;
#2429 = VERTEX_POINT ( 'NONE', #11011 ) ;
#2430 = B_SPLINE_CURVE_WITH_KNOTS ( 'NONE', 3,
 ( #1775, #12825, #891, #2084, #11638, #12747, #11790, #4246, #13945, #2008, #740, #818, #9335, #5606, #10453, #15306, #9263, #6882 ),
 .UNSPECIFIED., .F., .F.,
 ( 4, 2, 2, 2, 2, 2, 2, 2, 4 ),
 ( 0.003131918686235953507, 0.003523310662250245945, 0.003914702638264538383, 0.004306094614278830821, 0.004697486590293124126, 0.005088878566307415696, 0.005480270542321709001, 0.005871662518336001439, 0.006263054494350293877 ),
 .UNSPECIFIED. ) ;
#2431 = CARTESIAN_POINT ( 'NONE',  ( -5.317509234263937401, 2.779225709351033746, 11.63061695532135786 ) ) ;
#2432 = CARTESIAN_POINT ( 'NONE',  ( -0.1323602877611484707, -6.000000000000003553, 12.49999999999998401 ) ) ;
#2433 = ADVANCED_FACE ( 'NONE', ( #14677 ), #9904, .T. ) ;
#2435 = EDGE_LOOP ( 'NONE', ( #12638, #13087 ) ) ;
#2434 = CARTESIAN_POINT ( 'NONE',  ( -6.911788849595090767E-16, 187.7999999999999829, 9.500000000000001776 ) ) ;
#2436 = CARTESIAN_POINT ( 'NONE',  ( -2.283493650000000041, 0.000000000000000000, 1.925000001638712321 ) ) ;
#2437 = FACE_OUTER_BOUND ( 'NONE', #2227, .T. ) ;
#2438 = B_SPLINE_CURVE_WITH_KNOTS ( 'NONE', 3,
 ( #11494, #668, #14793, #12393, #10236, #10391, #5620, #11728, #15164, #754, #9052, #14038, #15240, #6895, #3879, #6817, #12690, #4261 ),
 .UNSPECIFIED., .F., .F.,
 ( 4, 2, 2, 2, 2, 2, 2, 2, 4 ),
 ( 0.000000000000000000, 0.0003914357524127461845, 0.0007828715048254923691, 0.001174307257238238608, 0.001565743009650985822, 0.001957178762063732820, 0.002348614514476479818, 0.002740050266889227683, 0.003131486019301974247 ),
 .UNSPECIFIED. ) ;
#2439 = CARTESIAN_POINT ( 'NONE',  ( -4.286401442266639883, 4.198423832313084247, 11.36938304467859417 ) ) ;
#2440 = CARTESIAN_POINT ( 'NONE',  ( 3.796994071234844259E-16, -2.066987299999999639, 1.650000001092474911 ) ) ;
#2441 = CARTESIAN_POINT ( 'NONE',  ( 5.375913338529100471, -2.664979843780421298, 4.495710796379801977 ) ) ;
#2442 = SHAPE_REPRESENTATION_RELATIONSHIP ( 'NONE' , 'NONE' ,  #3660, #4613 ) ;
#2443 = CARTESIAN_POINT ( 'NONE',  ( -0.7995524673975431540, -6.199337389817270783, 31.61453679452459653 ) ) ;
#2444 = CARTESIAN_POINT ( 'NONE',  ( 2.500000000000000444, 184.0500000000000114, 5.964466094067262247 ) ) ;
#2445 = CARTESIAN_POINT ( 'NONE',  ( -5.940390500375820615, 6.474944468551430354, 24.49999999999999289 ) ) ;
#2446 = CARTESIAN_POINT ( 'NONE',  ( 1.312858199469658427, 228.7505821040874139, 8.407114783769989330 ) ) ;
#2447 = CARTESIAN_POINT ( 'NONE',  ( -2.066987299999999639, 0.000000000000000000, 0.6500000010924747995 ) ) ;
#2448 = EDGE_CURVE ( 'NONE', #1252, #7643, #15534, .T. ) ;
#2449 = CARTESIAN_POINT ( 'NONE',  ( -1.035533905932737753, 2.500000000000000444, 1.550000000000000266 ) ) ;
#2450 = ORIENTED_EDGE ( 'NONE', *, *, #12036, .T. ) ;
#2452 = CARTESIAN_POINT ( 'NONE',  ( -6.268043809681822509E-16, 188.0499999989075093, 9.066987300000000971 ) ) ;
#2451 = PRODUCT ( 'slotted cheese head screw_iso_ISO 1207 - M3 x 5 - 5N', 'slotted cheese head screw_iso_ISO 1207 - M3 x 5 - 5N', '', ( #3281 ) ) ;
#2453 = CARTESIAN_POINT ( 'NONE',  ( 2.066987300000000527, 185.0499999989075093, 7.000000000000000000 ) ) ;
#2454 = CARTESIAN_POINT ( 'NONE',  ( -1.965116437629976787E-16, 189.2499999989075263, 4.933012699999999029 ) ) ;
#2455 = ORIENTED_EDGE ( 'NONE', *, *, #4255, .T. ) ;
#2456 = CARTESIAN_POINT ( 'NONE',  ( -4.286401442266675410, -4.198423832313046944, 24.49999999999999289 ) ) ;
#2457 = DIRECTION ( 'NONE',  ( 0.000000000000000000, 0.000000000000000000, -1.000000000000000000 ) ) ;
#2458 = DIRECTION ( 'NONE',  ( -0.5877852522924685852, -0.8090169943749507819, 0.000000000000000000 ) ) ;
#2459 = VECTOR ( 'NONE', #14120, 1000.000000000000114 ) ;
#2460 = CARTESIAN_POINT ( 'NONE',  ( 0.000000000000000000, 186.5669965222008386, 9.317226423031119253 ) ) ;
#2461 = CARTESIAN_POINT ( 'NONE',  ( -2.066987300000001415, 188.6999999989075150, 7.856174172912944620 ) ) ;
#2462 = CARTESIAN_POINT ( 'NONE',  ( 3.011899281037340614, 5.190111395030321262, 18.80022217383878669 ) ) ;
#2463 = CARTESIAN_POINT ( 'NONE',  ( 4.592425496802573972E-16, -2.500000000000000000, -2.799999997815050268 ) ) ;
#2464 = CARTESIAN_POINT ( 'NONE',  ( 0.000000000000000000, 0.000000000000000000, 2.500000000000000000 ) ) ;
#2465 = CARTESIAN_POINT ( 'NONE',  ( 5.866817325727516241, -1.260653813891924546, 31.80022217383877248 ) ) ;
#2466 = CARTESIAN_POINT ( 'NONE',  ( -3.883588957979242640, 4.898466244118940160, 30.02622717124731722 ) ) ;
#2467 = CARTESIAN_POINT ( 'NONE',  ( 5.915699123067152954, 1.003533581835587274, 4.496102049840166259 ) ) ;
#2468 =( BOUNDED_CURVE ( )  B_SPLINE_CURVE ( 2, ( #14032, #1782, #4490, #3141, #11647, #12915, #7993, #749, #4256, #11488, #5614, #7837, #4176, #12685, #4417 ),
 .UNSPECIFIED., .F., .F. ) 
 B_SPLINE_CURVE_WITH_KNOTS ( ( 3, 2, 2, 2, 2, 2, 2, 3 ),
 ( 0.7678695020645334157, 0.7857142857142856984, 0.8035714285714286031, 0.8214285714285713969, 0.8392857142857143016, 0.8571428571428570953, 0.8750000000000000000, 0.8928571428571429047 ),
 .UNSPECIFIED. ) 
 CURVE ( )  GEOMETRIC_REPRESENTATION_ITEM ( )  RATIONAL_B_SPLINE_CURVE ( ( 0.9998947045988972882, 0.9239322166753706211, 1.000000000000000000, 0.9238795325112867385, 1.000000000000000000, 0.9238795325112867385, 1.000000000000000000, 0.9238795325112867385, 1.000000000000000000, 0.9238795325112867385, 1.000000000000000000, 0.9238795325112867385, 1.000000000000000000, 0.9238795325112867385, 1.000000000000000000 ) ) 
 REPRESENTATION_ITEM ( '' )  );
#2469 = CARTESIAN_POINT ( 'NONE',  ( -5.915653884842715371, 1.003805156977378932, 30.49560239355786351 ) ) ;
#2470 = B_SPLINE_CURVE_WITH_KNOTS ( 'NONE', 3,
 ( #11598, #11910, #13026, #12949, #11827, #697, #15191, #7947, #13105, #14140, #3170, #4289, #12787, #2205, #9379, #7074, #14217, #9153 ),
 .UNSPECIFIED., .F., .F.,
 ( 4, 2, 2, 2, 2, 2, 2, 2, 4 ),
 ( 0.000000000000000000, 0.0003914898357794963568, 0.0007829796715589927136, 0.001174469507338488962, 0.001565959343117985427, 0.001957449178897482760, 0.002348939014676979225, 0.002740428850456475256, 0.003131918686235972155 ),
 .UNSPECIFIED. ) ;
#2471 = ORIENTED_EDGE ( 'NONE', *, *, #4839, .F. ) ;
#2472 = ORIENTED_EDGE ( 'NONE', *, *, #12897, .F. ) ;
#2473 = ORIENTED_EDGE ( 'NONE', *, *, #2427, .F. ) ;
#2474 = CARTESIAN_POINT ( 'NONE',  ( -2.668367453516892418, 5.373994336898001656, 24.63239388001634111 ) ) ;
#2475 = VERTEX_POINT ( 'NONE', #3124 ) ;
#2476 = B_SPLINE_CURVE_WITH_KNOTS ( 'NONE', 3,
 ( #10656, #2133, #4381, #11764, #5733, #4455, #11610, #14299, #709, #7959, #8119, #9310, #14225, #3408, #12799, #15437, #9387, #10427 ),
 .UNSPECIFIED., .F., .F.,
 ( 4, 2, 2, 2, 2, 2, 2, 2, 4 ),
 ( 0.003131486019301992028, 0.003522824630466699167, 0.003914163241631405873, 0.004305501852796113013, 0.004696840463960820153, 0.005088179075125527293, 0.005479517686290232698, 0.005870856297454939837, 0.006262194908619645242 ),
 .UNSPECIFIED. ) ;
#2477 = PRODUCT_DEFINITION_SHAPE ( 'NONE', 'NONE',  #15744 ) ;
#2478 = CARTESIAN_POINT ( 'NONE',  ( 1.461580736456472573, 1.461580736456472795, 1.750000001092474999 ) ) ;
#2479 = CARTESIAN_POINT ( 'NONE',  ( -6.105925084677672920, -1.337450587213226072, 12.29933148907575990 ) ) ;
#2480 = AXIS2_PLACEMENT_3D ( 'NONE', #9038, #2899, #426 ) ;
#2481 = DIRECTION ( 'NONE',  ( 0.000000000000000000, 0.000000000000000000, 1.000000000000000000 ) ) ;
#2482 = CARTESIAN_POINT ( 'NONE',  ( -1.461580736456473018, 187.1499999989075320, 5.538419263543527649 ) ) ;
#2483 = CARTESIAN_POINT ( 'NONE',  ( -1.035533905932737753, 2.500000000000000444, 2.350000000000000533 ) ) ;
#2484 = AXIS2_PLACEMENT_3D ( 'NONE', #13916, #481, #8852 ) ;
#2485 = CARTESIAN_POINT ( 'NONE',  ( -5.866923913994654072, 1.260079467906490391, 31.79952054102715309 ) ) ;
#2486 = CARTESIAN_POINT ( 'NONE',  ( 4.267558728637244059, -4.217879122113751933, 31.26382603205595601 ) ) ;
#2487 = CARTESIAN_POINT ( 'NONE',  ( -2.066987299999999639, 0.000000000000000000, 1.450000001092474955 ) ) ;
#2488 = FACE_OUTER_BOUND ( 'NONE', #14030, .T. ) ;
#2489 = CARTESIAN_POINT ( 'NONE',  ( -2.995192278888715975, 227.2265329420484647, 7.142163989385624134 ) ) ;
#2490 = CARTESIAN_POINT ( 'NONE',  ( 6.176542424588107316, 0.9554180641286319497, 5.130606907234995795 ) ) ;
#2491 = ORIENTED_EDGE ( 'NONE', *, *, #11796, .F. ) ;
#2492 = VERTEX_POINT ( 'NONE', #7977 ) ;
#2493 = VECTOR ( 'NONE', #6616, 1000.000000000000114 ) ;
#2494 = ORIENTED_EDGE ( 'NONE', *, *, #13420, .F. ) ;
#2495 = VERTEX_POINT ( 'NONE', #9179 ) ;
#2496 = CARTESIAN_POINT ( 'NONE',  ( 0.9085682363223165359, 189.0000000000000000, 9.333306381406472951 ) ) ;
#2497 = AXIS2_PLACEMENT_3D ( 'NONE', #1809, #12555, #7869 ) ;
#2498 = EDGE_CURVE ( 'NONE', #3136, #2410, #6811, .T. ) ;
#2499 = CARTESIAN_POINT ( 'NONE',  ( 0.000000000000000000, -0.001000000000000132727, -13.50000000000000000 ) ) ;
#2500 = EDGE_CURVE ( 'NONE', #7716, #4668, #5113, .T. ) ;
#2501 = CARTESIAN_POINT ( 'NONE',  ( 2.668367453516645504, -5.373994336898123336, 11.49999999999998224 ) ) ;
#2502 = UNCERTAINTY_MEASURE_WITH_UNIT (LENGTH_MEASURE( 1.000000000000000082E-05 ), #2041, 'distance_accuracy_value', 'NONE');
#2503 = CARTESIAN_POINT ( 'NONE',  ( 4.435347140100927454, -4.403429997944614982, 24.36762589283694069 ) ) ;
#2504 = CYLINDRICAL_SURFACE ( 'NONE', #14010, 3.000000000000000000 ) ;
#2505 = CARTESIAN_POINT ( 'NONE',  ( -4.344762547369766637, 4.493114738039160727, 10.99691356133951992 ) ) ;
#2506 = CARTESIAN_POINT ( 'NONE',  ( 0.6152055445547642831, -5.969096820685141580, 18.79904968670266996 ) ) ;
#2507 = CARTESIAN_POINT ( 'NONE',  ( -2.500000000000000888, 188.3999999999999773, 7.000000000000000000 ) ) ;
#2508 = EDGE_CURVE ( 'NONE', #1119, #4626, #12680, .T. ) ;
#2509 = CARTESIAN_POINT ( 'NONE',  ( 6.805491029613696752E-14, 26.00000000000000355, -9.750000000000003553 ) ) ;
#2510 = MECHANICAL_DESIGN_GEOMETRIC_PRESENTATION_REPRESENTATION (  '', ( #7844 ), #724 ) ;
#2511 = CARTESIAN_POINT ( 'NONE',  ( 2.500000000000000444, 187.8499999978150470, 8.035533905932739529 ) ) ;
#2512 = AXIS2_PLACEMENT_3D ( 'NONE', #12106, #1207, #6078 ) ;
#2513 = CARTESIAN_POINT ( 'NONE',  ( 2.961752869269595134, 227.1327854310254111, 6.866142280206398496 ) ) ;
#2514 = CARTESIAN_POINT ( 'NONE',  ( 5.935543223013856284, 0.8771126767606806096, 11.49999999999998224 ) ) ;
#2515 = CARTESIAN_POINT ( 'NONE',  ( -0.8793070671816629602, 189.7084256268280456, 10.26238677585280179 ) ) ;
#2516 = VERTEX_POINT ( 'NONE', #1843 ) ;
#2517 = DIRECTION ( 'NONE',  ( -1.000000000000000000, 0.000000000000000000, 0.000000000000000000 ) ) ;
#2518 = CARTESIAN_POINT ( 'NONE',  ( -2.897581130414634077E-17, 9.750000000000003553, 0.000000000000000000 ) ) ;
#2519 = CARTESIAN_POINT ( 'NONE',  ( 5.409423237179071364, 2.597448116730906253, 25.11561732698605098 ) ) ;
#2520 = CARTESIAN_POINT ( 'NONE',  ( 0.000000000000000000, 2.000000000000000000, 0.000000000000000000 ) ) ;
#2521 = CARTESIAN_POINT ( 'NONE',  ( 1.129999918305732987, 226.3961343599838756, 4.695842443849920222 ) ) ;
#2522 = DIRECTION ( 'NONE',  ( 0.000000000000000000, 0.000000000000000000, 1.000000000000000000 ) ) ;
#2523 = CARTESIAN_POINT ( 'NONE',  ( 2.066987299999999639, 2.531329380823229670E-16, 0.2500000010924748328 ) ) ;
#2524 = DIRECTION ( 'NONE',  ( 0.000000000000000000, 0.000000000000000000, 1.000000000000000000 ) ) ;
#2525 = CARTESIAN_POINT ( 'NONE',  ( -0.8730628416137050651, -6.188929913094965762, 30.49504929893117122 ) ) ;
#2526 = CARTESIAN_POINT ( 'NONE',  ( 1.035533905932738197, 187.7800000002184788, 9.500000000000003553 ) ) ;
#2527 = FACE_BOUND ( 'NONE', #12681, .T. ) ;
#2529 = CARTESIAN_POINT ( 'NONE',  ( 1.814481968427068992, 227.9916212483514641, 6.215192544112370321 ) ) ;
#2528 = VECTOR ( 'NONE', #10347, 1000.000000000000000 ) ;
#2530 = CARTESIAN_POINT ( 'NONE',  ( 0.8561741729129452860, 2.066987299999999639, -0.3999999989075251339 ) ) ;
#2531 = LINE ( 'NONE', #7386, #7975 ) ;
#2532 = VECTOR ( 'NONE', #3932, 1000.000000000000000 ) ;
#2533 = ORIENTED_EDGE ( 'NONE', *, *, #557, .T. ) ;
#2534 = CARTESIAN_POINT ( 'NONE',  ( 2.066987300000000083, 187.3999999989075320, 7.856174172912946396 ) ) ;
#2535 = EDGE_CURVE ( 'NONE', #9028, #13870, #1855, .T. ) ;
#2536 = CARTESIAN_POINT ( 'NONE',  ( 0.8561741729129461742, 184.8999999989075320, 9.066987300000000971 ) ) ;
#2537 = CARTESIAN_POINT ( 'NONE',  ( 5.375886393124428508, 2.665038680141196270, 23.99560239355785640 ) ) ;
#2539 = ORIENTED_EDGE ( 'NONE', *, *, #6410, .F. ) ;
#2538 = CARTESIAN_POINT ( 'NONE',  ( 2.817313151351089839, 5.579000502529481764, 31.00000000000000000 ) ) ;
#2540 = CARTESIAN_POINT ( 'NONE',  ( 9.750000000000003553, 182.0000000000000000, -1.499999999999897415 ) ) ;
#2541 = CARTESIAN_POINT ( 'NONE',  ( 0.6139731865241975228, -6.220476368274032275, 23.69975545601931799 ) ) ;
#2542 = EDGE_CURVE ( 'NONE', #3463, #3038, #10755, .T. ) ;
#2543 = CARTESIAN_POINT ( 'NONE',  ( 5.999999999999999112, 215.7452399395091618, 13.29567785264566027 ) ) ;
#2544 = CARTESIAN_POINT ( 'NONE',  ( -2.369853004795346330, 188.9999999999999716, 6.157114161223693038 ) ) ;
#2545 = CARTESIAN_POINT ( 'NONE',  ( 5.935543223013889147, -0.8771126767604601193, 24.49999999999999289 ) ) ;
#2546 = CARTESIAN_POINT ( 'NONE',  ( 2.500000000000000444, 1.035533905932737975, -2.549999997815051156 ) ) ;
#2547 = DIRECTION ( 'NONE',  ( -0.9510565162951544194, 0.3090169943749447312, 0.000000000000000000 ) ) ;
#2548 = CARTESIAN_POINT ( 'NONE',  ( 5.620786884546307149, -2.102685372472853143, 31.97358595436693918 ) ) ;
#2549 = CARTESIAN_POINT ( 'NONE',  ( -0.2623718222033848413, -6.245654667075791089, 17.02627829713834018 ) ) ;
#2550 = CARTESIAN_POINT ( 'NONE',  ( -9.750000000000003553, 3.401296724241641415E-14, 0.000000000000000000 ) ) ;
#2551 = CARTESIAN_POINT ( 'NONE',  ( 5.409423237179016297, 2.597448116731026602, 12.11561732698603855 ) ) ;
#2552 = EDGE_LOOP ( 'NONE', ( #4370, #493, #15450, #8595 ) ) ;
#2553 =( BOUNDED_CURVE ( )  B_SPLINE_CURVE ( 2, ( #13878, #2991, #6739, #1865, #9276, #10311, #14113, #6662, #5698 ),
 .UNSPECIFIED., .F., .F. ) 
 B_SPLINE_CURVE_WITH_KNOTS ( ( 3, 2, 2, 2, 3 ),
 ( 0.07142857142857142461, 0.08928571428571428770, 0.1071428571428571369, 0.1250000000000000000, 0.1428571428571428492 ),
 .UNSPECIFIED. ) 
 CURVE ( )  GEOMETRIC_REPRESENTATION_ITEM ( )  RATIONAL_B_SPLINE_CURVE ( ( 1.000000000000000000, 0.9238795325112867385, 1.000000000000000000, 0.9238795325112867385, 1.000000000000000000, 0.9238795325112867385, 1.000000000000000000, 0.9238795325112867385, 1.000000000000000000 ) ) 
 REPRESENTATION_ITEM ( '' )  );
#2554 = ORIENTED_EDGE ( 'NONE', *, *, #1166, .F. ) ;
#2555 = ORIENTED_EDGE ( 'NONE', *, *, #7831, .F. ) ;
#2556 = DIRECTION ( 'NONE',  ( -6.123233995736766036E-17, 1.000000000000000000, 0.000000000000000000 ) ) ;
#2557 = ORIENTED_EDGE ( 'NONE', *, *, #14453, .T. ) ;
#2558 = CARTESIAN_POINT ( 'NONE',  ( 2.066987300000000083, -0.8561741729129449530, 0.8000000010924747107 ) ) ;
#2559 = CARTESIAN_POINT ( 'NONE',  ( 9.750000000000003553, 22.00000000000000000, 1.020968533498575335E-13 ) ) ;
#2560 = CARTESIAN_POINT ( 'NONE',  ( 6.155973317223280894, 1.081218830693758903, 31.50308643866045344 ) ) ;
#2561 = CARTESIAN_POINT ( 'NONE',  ( 1.461580736456472351, 188.3499999989074922, 8.461580736456474128 ) ) ;
#2562 = CARTESIAN_POINT ( 'NONE',  ( 4.592425496802573972E-16, -2.500000000000000000, 0.2999999999999999334 ) ) ;
#2563 = CARTESIAN_POINT ( 'NONE',  ( -5.375605342016520183, 2.665598297262264715, 31.50312048902376816 ) ) ;
#2564 = CARTESIAN_POINT ( 'NONE',  ( -7.799024015210663130, -1.482594289697217294, 5.000000000000004441 ) ) ;
#2565 = CARTESIAN_POINT ( 'NONE',  ( 0.8561741729129451750, 2.066987299999999639, -1.399999998907525800 ) ) ;
#2566 = CARTESIAN_POINT ( 'NONE',  ( 6.123233995736766282E-16, -6.250000000000000888, 5.000000000000004441 ) ) ;
#2567 = CARTESIAN_POINT ( 'NONE',  ( -2.842171547016528965, 226.9791356524935395, 6.413666598675894726 ) ) ;
#2568 = ORIENTED_EDGE ( 'NONE', *, *, #6631, .F. ) ;
#2569 = ORIENTED_EDGE ( 'NONE', *, *, #15274, .T. ) ;
#2570 = ORIENTED_EDGE ( 'NONE', *, *, #10476, .T. ) ;
#2571 = CIRCLE ( 'NONE', #6652, 2.500000000000000000 ) ;
#2572 = DIRECTION ( 'NONE',  ( -0.000000000000000000, 1.000000000000000000, -0.000000000000000000 ) ) ;
#2573 = CARTESIAN_POINT ( 'NONE',  ( 2.817313151351107159, 5.579000502529472882, 4.869393092765015751 ) ) ;
#2574 = CARTESIAN_POINT ( 'NONE',  ( -0.2624013748573160165, -5.995472630654518298, 4.026285596910829767 ) ) ;
#2575 = CARTESIAN_POINT ( 'NONE',  ( -4.267838854167186113, -4.217593933790326766, 18.26239891805597537 ) ) ;
#2576 = CARTESIAN_POINT ( 'NONE',  ( 0.7995298244855156833, 5.947211616899241271, 12.11456014619857946 ) ) ;
#2577 = DIRECTION ( 'NONE',  ( 0.000000000000000000, 0.000000000000000000, -1.000000000000000000 ) ) ;
#2578 = CARTESIAN_POINT ( 'NONE',  ( 5.409274167810689704, -2.597759609440573492, 12.11519382448850557 ) ) ;
#2579 = CARTESIAN_POINT ( 'NONE',  ( 0.000000000000000000, 182.0000000000000000, 0.000000000000000000 ) ) ;
#2580 = LINE ( 'NONE', #7363, #10244 ) ;
#2581 = DIRECTION ( 'NONE',  ( 1.000000000000000000, 0.000000000000000000, 0.000000000000000000 ) ) ;
#2582 = PRODUCT_DEFINITION_SHAPE ( 'NONE', 'NONE',  #3028 ) ;
#2583 = AXIS2_PLACEMENT_3D ( 'NONE', #10617, #9196, #6737 ) ;
#2584 = CARTESIAN_POINT ( 'NONE',  ( -1.456896669277396583E-16, 188.8999999978150584, 4.500000000000000000 ) ) ;
#2585 = CARTESIAN_POINT ( 'NONE',  ( 2.923766376317260551, 227.0711491207812855, 6.684645050985161596 ) ) ;
#2586 = EDGE_CURVE ( 'NONE', #6402, #4624, #13832, .T. ) ;
#2587 = CARTESIAN_POINT ( 'NONE',  ( -0.4847600579890295469, 189.7005989459862860, 10.35649496429148897 ) ) ;
#2588 = VERTEX_POINT ( 'NONE', #4558 ) ;
#2589 = CARTESIAN_POINT ( 'NONE',  ( -3.311384659207134984, 5.004923837169420686, 5.973585954366940953 ) ) ;
#2590 = CARTESIAN_POINT ( 'NONE',  ( -5.558508435838217743, 2.857531096718874952, 30.86936067245787640 ) ) ;
#2591 = CARTESIAN_POINT ( 'NONE',  ( -1.035533905932737753, 2.500000000000000444, -0.8500000000000001998 ) ) ;
#2592 = DIRECTION ( 'NONE',  ( 0.000000000000000000, 0.000000000000000000, -1.000000000000000000 ) ) ;
#2593 = CARTESIAN_POINT ( 'NONE',  ( 0.000000000000000000, 0.000000000000000000, 2.500000000000000000 ) ) ;
#2594 = CARTESIAN_POINT ( 'NONE',  ( -3.061616997868386099E-16, 189.0000000000000000, -7.000000000000000000 ) ) ;
#2595 = CARTESIAN_POINT ( 'NONE',  ( 0.8561741729129451750, 2.066987299999999639, 2.000000001092475443 ) ) ;
#2596 = CARTESIAN_POINT ( 'NONE',  ( -2.931212650151840293, 5.520239928492722825, 23.99574050496988065 ) ) ;
#2597 = LINE ( 'NONE', #1396, #109 ) ;
#2598 = CARTESIAN_POINT ( 'NONE',  ( -2.500000000000000888, 187.5300000002185072, 7.000000000000000000 ) ) ;
#2599 = CARTESIAN_POINT ( 'NONE',  ( 0.000000000000000000, 0.000000000000000000, 5.000000000000004441 ) ) ;
#2600 = EDGE_CURVE ( 'NONE', #6522, #6002, #2249, .T. ) ;
#2601 = CARTESIAN_POINT ( 'NONE',  ( 0.06495987523896813720, 228.9118724015956730, 8.872930362369002566 ) ) ;
#2602 = CARTESIAN_POINT ( 'NONE',  ( 1.461580736456473018, -1.461580736456472573, -1.449999998907525178 ) ) ;
#2603 = AXIS2_PLACEMENT_3D ( 'NONE', #14738, #13220, #3825 ) ;
#2604 = DIRECTION ( 'NONE',  ( 0.000000000000000000, 0.000000000000000000, -1.000000000000000000 ) ) ;
#2605 = ORIENTED_EDGE ( 'NONE', *, *, #14901, .F. ) ;
#2606 = CARTESIAN_POINT ( 'NONE',  ( -1.461580736456472351, -1.461580736456473018, 0.5500000010924748217 ) ) ;
#2607 = B_SPLINE_CURVE_WITH_KNOTS ( 'NONE', 3,
 ( #12396, #14796, #8755, #7630, #10099, #13587, #1496, #11207, #11285, #5015, #308, #382, #5169, #10022, #3960, #8834, #2269, #7140 ),
 .UNSPECIFIED., .F., .F.,
 ( 4, 2, 2, 2, 2, 2, 2, 2, 4 ),
 ( 0.003131918686235974757, 0.003523310662250265460, 0.003914702638264555730, 0.004306094614278846433, 0.004697486590293137136, 0.005088878566307427839, 0.005480270542321717675, 0.005871662518336008378, 0.006263054494350299081 ),
 .UNSPECIFIED. ) ;
#2608 = CARTESIAN_POINT ( 'NONE',  ( -2.066987300000000971, 184.5999999989074922, 6.143825827087054492 ) ) ;
#2609 = CARTESIAN_POINT ( 'NONE',  ( -3.735642931251144994, 4.696778275484382092, 18.97408052783099563 ) ) ;
#2610 = EDGE_CURVE ( 'NONE', #3990, #13214, #1100, .T. ) ;
#2612 = EDGE_LOOP ( 'NONE', ( #12888, #3745 ) ) ;
#2611 = CARTESIAN_POINT ( 'NONE',  ( -1.500000000000000000, 0.000000000000000000, 2.500000000000000000 ) ) ;
#2613 = CARTESIAN_POINT ( 'NONE',  ( -3.311384659207235792, -5.004923837169353185, 23.52641404563305016 ) ) ;
#2614 = CARTESIAN_POINT ( 'NONE',  ( 5.940390500375496430, 6.474944468551661281, 11.49999999999998224 ) ) ;
#2615 = AXIS2_PLACEMENT_3D ( 'NONE', #10996, #9813, #12262 ) ;
#2616 = EDGE_CURVE ( 'NONE', #7910, #4035, #11161, .T. ) ;
#2617 = CARTESIAN_POINT ( 'NONE',  ( 5.649053410273082498, -2.675685104943239523, 31.61517780375841369 ) ) ;
#2618 = CARTESIAN_POINT ( 'NONE',  ( 0.000000000000000000, 215.7452399395091049, 13.29567785264566027 ) ) ;
#2619 = CARTESIAN_POINT ( 'NONE',  ( 0.8561741729129458411, 188.8999999989075320, 9.066987300000000971 ) ) ;
#2620 = CARTESIAN_POINT ( 'NONE',  ( 5.317509234264064411, -2.779225709350791274, 24.49999999999999289 ) ) ;
#2621 = CARTESIAN_POINT ( 'NONE',  ( 2.500000000000000444, -1.035533905932737309, -1.849999997815050090 ) ) ;
#2622 = DIRECTION ( 'NONE',  ( 0.000000000000000000, 0.000000000000000000, 1.000000000000000000 ) ) ;
#2623 = CARTESIAN_POINT ( 'NONE',  ( 0.000000000000000000, 0.000000000000000000, 36.00000000000000711 ) ) ;
#2624 = CARTESIAN_POINT ( 'NONE',  ( -5.317509234263939177, 2.779225709351033302, 11.49999999999998224 ) ) ;
#2625 = CARTESIAN_POINT ( 'NONE',  ( -5.317509234263898321, -2.779225709351108797, 11.63064961348853465 ) ) ;
#2626 = CARTESIAN_POINT ( 'NONE',  ( 3.922396193918885832, 4.541970110199584632, 23.62619317285288645 ) ) ;
#2627 = ORIENTED_EDGE ( 'NONE', *, *, #10989, .T. ) ;
#2628 = CARTESIAN_POINT ( 'NONE',  ( -1.461580736456473462, 187.3499999989075206, 8.461580736456472351 ) ) ;
#2629 = ADVANCED_FACE ( 'NONE', ( #9885 ), #6153, .T. ) ;
#2630 = AXIS2_PLACEMENT_3D ( 'NONE', #6474, #15129, #11308 ) ;
#2631 = ORIENTED_EDGE ( 'NONE', *, *, #1073, .T. ) ;
#2632 = ORIENTED_EDGE ( 'NONE', *, *, #12161, .F. ) ;
#2633 = CARTESIAN_POINT ( 'NONE',  ( -5.935543223013816316, -0.8771126767609508379, 24.49999999999999289 ) ) ;
#2634 = ORIENTED_EDGE ( 'NONE', *, *, #4191, .F. ) ;
#2635 = CARTESIAN_POINT ( 'NONE',  ( -0.8561741729129455081, 2.066987299999999639, -1.299999998907525267 ) ) ;
#2636 = B_SPLINE_CURVE_WITH_KNOTS ( 'NONE', 3,
 ( #10897, #7395, #13508, #1181, #2617, #4776, #1448, #3648, #229, #7472, #12238, #1339, #11571, #597, #12921, #1492, #13960, #4182 ),
 .UNSPECIFIED., .F., .F.,
 ( 4, 2, 2, 2, 2, 2, 2, 2, 4 ),
 ( 0.000000000000000000, 0.0003914357524127471061, 0.0007828715048254942122, 0.001174307257238241427, 0.001565743009650988424, 0.001957178762063735422, 0.002348614514476482854, 0.002740050266889229851, 0.003131486019301976849 ),
 .UNSPECIFIED. ) ;
#2637 = CARTESIAN_POINT ( 'NONE',  ( -5.558508435838158235, -2.857531096718993524, 11.63063932754212892 ) ) ;
#2638 = CARTESIAN_POINT ( 'NONE',  ( -1.735141101668105090, 228.0777902684043852, 9.646862769529031212 ) ) ;
#2639 = LINE ( 'NONE', #12495, #7435 ) ;
#2640 = VECTOR ( 'NONE', #3726, 1000.000000000000000 ) ;
#2641 = CARTESIAN_POINT ( 'NONE',  ( 2.500000000000000000, 3.061616997868383141E-16, 0.5000000000000000000 ) ) ;
#2642 =( REPRESENTATION_RELATIONSHIP ('NONE','NONE', #11191, #4596 ) REPRESENTATION_RELATIONSHIP_WITH_TRANSFORMATION ( #10201 )SHAPE_REPRESENTATION_RELATIONSHIP( ) );
#2643 = FACE_OUTER_BOUND ( 'NONE', #6380, .T. ) ;
#2644 = ITEM_DEFINED_TRANSFORMATION ( 'NONE', 'NONE', #11369,  #14201 ) ;
#2645 = CARTESIAN_POINT ( 'NONE',  ( 4.267936573529233613, 4.217499624512214496, 5.262290378359326226 ) ) ;
#2646 = CARTESIAN_POINT ( 'NONE',  ( -1.265664690411614835E-16, 2.066987299999999639, -2.949999998907525178 ) ) ;
#2647 = CARTESIAN_POINT ( 'NONE',  ( 6.106056299406760424, -1.336851112280608378, 10.70112161576659560 ) ) ;
#2648 = CARTESIAN_POINT ( 'NONE',  ( -1.747606509155581689, 226.5054486174500994, 5.018058692477180394 ) ) ;
#2649 = VERTEX_POINT ( 'NONE', #6309 ) ;
#2650 = ORIENTED_EDGE ( 'NONE', *, *, #3508, .F. ) ;
#2651 = EDGE_CURVE ( 'NONE', #9577, #15709, #4254, .T. ) ;
#2652 = ORIENTED_EDGE ( 'NONE', *, *, #4161, .T. ) ;
#2653 = CARTESIAN_POINT ( 'NONE',  ( -4.000000000000002665, 184.0000000000000000, -7.000000000000000000 ) ) ;
#2654 = CARTESIAN_POINT ( 'NONE',  ( 3.780072143464216605, 4.979057943639748629, 3.999917806784441865 ) ) ;
#2655 = CARTESIAN_POINT ( 'NONE',  ( 0.8738239080080354437, 6.188820299975593464, 5.503557957101424591 ) ) ;
#2656 = CARTESIAN_POINT ( 'NONE',  ( 0.5044069930203494145, -5.979990686694992341, 31.87335743227903606 ) ) ;
#2657 = CARTESIAN_POINT ( 'NONE',  ( 0.1306171417089282139, 6.000000000000000000, 10.49999999999998401 ) ) ;
#2658 = CARTESIAN_POINT ( 'NONE',  ( -5.861467994999758346E-16, 186.0999999978150754, 9.500000000000001776 ) ) ;
#2659 = DIRECTION ( 'NONE',  ( -0.000000000000000000, 1.000000000000000000, -0.000000000000000000 ) ) ;
#2660 = CARTESIAN_POINT ( 'NONE',  ( -6.155854678529491864, 1.081900940642012587, 5.504259495030091820 ) ) ;
#2661 = CARTESIAN_POINT ( 'NONE',  ( -2.668367453516813814, -5.373994336898041624, 24.49999999999999289 ) ) ;
#2662 = CARTESIAN_POINT ( 'NONE',  ( -9.750000000000003553, 26.00000000000000355, -3.401296724241641415E-14 ) ) ;
#2663 = CARTESIAN_POINT ( 'NONE',  ( 1.767766952966369098, 187.2699999975965568, 5.232233047033630235 ) ) ;
#2664 = CARTESIAN_POINT ( 'NONE',  ( -1.786743523428754976, 227.9724114945277051, 6.159713679416685572 ) ) ;
#2665 = CARTESIAN_POINT ( 'NONE',  ( -2.809592974547592714, 227.6294044507834542, 8.327915135215583575 ) ) ;
#2666 = AXIS2_PLACEMENT_3D ( 'NONE', #1854, #8067, #9265 ) ;
#2667 = ADVANCED_FACE ( 'NONE', ( #12258 ), #7262, .F. ) ;
#2668 = CARTESIAN_POINT ( 'NONE',  ( -1.830453387431577816, 189.0000000012350938, 8.709453706375219539 ) ) ;
#2669 = ORIENTED_EDGE ( 'NONE', *, *, #6985, .T. ) ;
#2670 = CARTESIAN_POINT ( 'NONE',  ( 1.530808498934191324E-15, 182.0000000000000000, 12.49999999999999822 ) ) ;
#2671 = CARTESIAN_POINT ( 'NONE',  ( -6.172639027853100480, 0.9816353142772724638, 24.23774718278285789 ) ) ;
#2672 = DIRECTION ( 'NONE',  ( 0.000000000000000000, 0.000000000000000000, 1.000000000000000000 ) ) ;
#2673 = CARTESIAN_POINT ( 'NONE',  ( 5.770331821586383469, 2.404225004693643086, 30.12619944752605150 ) ) ;
#2674 = CARTESIAN_POINT ( 'NONE',  ( 2.903473946076591705, 227.5344354822965443, 8.048524736755723552 ) ) ;
#2675 = CARTESIAN_POINT ( 'NONE',  ( -4.435347140101024266, -4.403429997944519947, 31.00000000000000000 ) ) ;
#2676 = CARTESIAN_POINT ( 'NONE',  ( -1.767766952966369098, 1.767766952966369098, 1.599999999999999867 ) ) ;
#2677 = CARTESIAN_POINT ( 'NONE',  ( 5.665707375537461843, -1.979196487016705586, 3.999920388255239434 ) ) ;
#2678 = CIRCLE ( 'NONE', #4715, 2.500000000000000000 ) ;
#2679 = CARTESIAN_POINT ( 'NONE',  ( 6.768587589771821120E-14, -6.250000000000000888, 12.49999999999998401 ) ) ;
#2680 = CARTESIAN_POINT ( 'NONE',  ( 1.767766952966369098, 186.5000000000000000, 5.232233047033630235 ) ) ;
#2681 = CARTESIAN_POINT ( 'NONE',  ( -1.767766952966368432, -1.767766952966369320, -2.099999997815050090 ) ) ;
#2682 = CARTESIAN_POINT ( 'NONE',  ( 0.000000000000000000, 184.0000000000000000, -12.49999999999999822 ) ) ;
#2683 = CARTESIAN_POINT ( 'NONE',  ( -0.8561741729129458411, -2.066987299999999195, -1.599999998907525756 ) ) ;
#2684 = CARTESIAN_POINT ( 'NONE',  ( 3.568242062701468598, 5.132954954975548212, 12.50004906876531052 ) ) ;
#2685 = CARTESIAN_POINT ( 'NONE',  ( 9.750000000000003553, 184.0000000000000000, 1.020968533498575461E-13 ) ) ;
#2686 = CARTESIAN_POINT ( 'NONE',  ( -6.776263578034402713E-16, 188.8499999989074922, 9.066987300000000971 ) ) ;
#2687 = CARTESIAN_POINT ( 'NONE',  ( -5.746837578675960678, -1.729433780394401099, 18.99995053646221521 ) ) ;
#2688 = AXIS2_PLACEMENT_3D ( 'NONE', #8502, #3466, #1157 ) ;
#2690 = ORIENTED_EDGE ( 'NONE', *, *, #7017, .F. ) ;
#2689 = CARTESIAN_POINT ( 'NONE',  ( -0.8561741729129467293, 186.5999999989075206, 9.066987299999999195 ) ) ;
#2691 = CARTESIAN_POINT ( 'NONE',  ( -2.931156713028501670, -5.520271803279203304, 17.49563030319846746 ) ) ;
#2692 = EDGE_CURVE ( 'NONE', #6081, #8841, #1960, .T. ) ;
#2693 = CARTESIAN_POINT ( 'NONE',  ( 5.558508435838260375, -2.857531096718793240, 11.49999999999998224 ) ) ;
#2694 = EDGE_CURVE ( 'NONE', #10558, #13993, #8074, .T. ) ;
#2695 =( NAMED_UNIT ( * ) SI_UNIT ( $, .STERADIAN. ) SOLID_ANGLE_UNIT ( ) );
#2696 = CARTESIAN_POINT ( 'NONE',  ( -5.866984344570858489, 1.259800266528510182, 4.200681937418259793 ) ) ;
#2697 = CARTESIAN_POINT ( 'NONE',  ( -6.776263578034402713E-16, 188.8499999989074922, 9.066987300000000971 ) ) ;
#2698 = CARTESIAN_POINT ( 'NONE',  ( 5.746619684944337614, -1.730157667110624908, 25.50004932073311892 ) ) ;
#2699 = CARTESIAN_POINT ( 'NONE',  ( -1.767766952966368432, -1.767766952966369320, -2.099999997815050090 ) ) ;
#2700 = DIRECTION ( 'NONE',  ( -6.123233995736766036E-17, 1.000000000000000000, 0.000000000000000000 ) ) ;
#2701 = CARTESIAN_POINT ( 'NONE',  ( 0.8628399698974030807, 190.0753276663367330, 4.324387286082350457 ) ) ;
#2702 = ADVANCED_FACE ( 'NONE', ( #168, #5029, #1433, #8544, #3589, #11147 ), #8463, .T. ) ;
#2703 = CARTESIAN_POINT ( 'NONE',  ( -4.344762547369738215, 4.493114738039190925, 30.49691356133954301 ) ) ;
#2704 = CARTESIAN_POINT ( 'NONE',  ( 0.3133709289734071812, -0.3999999999999975797, 2.571515392583413107 ) ) ;
#2705 = CARTESIAN_POINT ( 'NONE',  ( -5.317509234263900098, -2.779225709351109241, 11.36938304467859417 ) ) ;
#2706 = ORIENTED_EDGE ( 'NONE', *, *, #113, .F. ) ;
#2707 = CARTESIAN_POINT ( 'NONE',  ( -1.461580736456473462, 186.5499999989075093, 8.461580736456472351 ) ) ;
#2708 = ORIENTED_EDGE ( 'NONE', *, *, #8523, .F. ) ;
#2709 = DIRECTION ( 'NONE',  ( 0.5877852522924802425, -0.8090169943749422332, 0.000000000000000000 ) ) ;
#2710 = ORIENTED_EDGE ( 'NONE', *, *, #6872, .F. ) ;
#2711 = CARTESIAN_POINT ( 'NONE',  ( -4.267992336621335703, 4.217442018459861330, 24.76194324003146008 ) ) ;
#2712 = FILL_AREA_STYLE ('',( #3685 ) ) ;
#2713 = AXIS2_PLACEMENT_3D ( 'NONE', #1872, #6669, #8091 ) ;
#2714 = ORIENTED_EDGE ( 'NONE', *, *, #11323, .F. ) ;
#2715 = CARTESIAN_POINT ( 'NONE',  ( 2.066987300000000083, -0.8561741729129449530, -1.599999998907525534 ) ) ;
#2716 = CARTESIAN_POINT ( 'NONE',  ( 2.500000000000000444, 1.035533905932737975, -1.850000000000000533 ) ) ;
#2717 = CARTESIAN_POINT ( 'NONE',  ( -1.839562682118536241, 190.0280088719464402, 4.838899882289354970 ) ) ;
#2718 = CARTESIAN_POINT ( 'NONE',  ( -1.461580736456473462, 188.9499999989075150, 8.461580736456472351 ) ) ;
#2719 = CARTESIAN_POINT ( 'NONE',  ( 1.035533905932737531, 2.500000000000000444, 0.6500000000000000222 ) ) ;
#2720 = FACE_OUTER_BOUND ( 'NONE', #14878, .T. ) ;
#2721 = ITEM_DEFINED_TRANSFORMATION ( 'NONE', 'NONE', #10108,  #14201 ) ;
#2722 = CARTESIAN_POINT ( 'NONE',  ( 2.848727059636091408, -5.281416301279826087, 31.61442521571938258 ) ) ;
#2723 = CARTESIAN_POINT ( 'NONE',  ( 0.8561741729129451750, 2.066987299999999639, -0.3999999989075250784 ) ) ;
#2724 = CARTESIAN_POINT ( 'NONE',  ( 6.176542424588128632, -0.9554180641284775177, 11.49999999999998224 ) ) ;
#2725 = CARTESIAN_POINT ( 'NONE',  ( -1.748661130334981051, 228.0746845563984095, 9.637707355516731411 ) ) ;
#2726 = ORIENTED_EDGE ( 'NONE', *, *, #10094, .T. ) ;
#2727 = ORIENTED_EDGE ( 'NONE', *, *, #1242, .T. ) ;
#2728 = VERTEX_POINT ( 'NONE', #13297 ) ;
#2729 = EDGE_CURVE ( 'NONE', #3463, #7351, #6098, .T. ) ;
#2730 = CARTESIAN_POINT ( 'NONE',  ( 5.487097279078454015, -2.429065649168769436, 30.20047945897283981 ) ) ;
#2731 = CARTESIAN_POINT ( 'NONE',  ( 2.208001385524885674, 189.0000000000000000, 8.182568187910820967 ) ) ;
#2732 = EDGE_LOOP ( 'NONE', ( #2226, #7584, #10910, #13634 ) ) ;
#2733 = PRODUCT_DEFINITION_FORMATION_WITH_SPECIFIED_SOURCE ( 'ANY', '', #2451, .NOT_KNOWN. ) ;
#2734 = CARTESIAN_POINT ( 'NONE',  ( -0.7988914244718240409, -5.947301735519284094, 4.384562891686187847 ) ) ;
#2735 = CARTESIAN_POINT ( 'NONE',  ( 0.8737888311110264539, -5.936248257219505220, 31.50344185141217679 ) ) ;
#2736 = LINE ( 'NONE', #14832, #3235 ) ;
#2737 = CARTESIAN_POINT ( 'NONE',  ( -1.035533905932739751, 187.6499999978150584, 9.500000000000000000 ) ) ;
#2738 = CARTESIAN_POINT ( 'NONE',  ( 2.500000000000000444, 185.4999999978150527, 7.000000000000000000 ) ) ;
#2739 = SURFACE_SIDE_STYLE ('',( #4002 ) ) ;
#2740 = EDGE_CURVE ( 'NONE', #10533, #8352, #14159, .T. ) ;
#2741 = CYLINDRICAL_SURFACE ( 'NONE', #14104, 1.000000000000000888 ) ;
#2742 = CARTESIAN_POINT ( 'NONE',  ( 0.8736516769108820801, -5.936271176698206808, 23.99606771578674369 ) ) ;
#2743 = CARTESIAN_POINT ( 'NONE',  ( -9.750000000000003553, 186.0000000000000000, -3.401296724241641415E-14 ) ) ;
#2744 = CARTESIAN_POINT ( 'NONE',  ( 9.486769009248163798E-17, 184.9699999975965454, 4.500000000000000000 ) ) ;
#2745 = CARTESIAN_POINT ( 'NONE',  ( -1.923034433439944513, 228.0917019039344495, 6.504231185664401949 ) ) ;
#2746 = CARTESIAN_POINT ( 'NONE',  ( -1.978640506925948062, 228.0159251728749155, 9.464911921216582869 ) ) ;
#2747 = AXIS2_PLACEMENT_3D ( 'NONE', #6769, #14144, #10650 ) ;
#2748 = CARTESIAN_POINT ( 'NONE',  ( -1.383648599222811360, 188.9999999995481517, 9.087128311603166253 ) ) ;
#2749 = ORIENTED_EDGE ( 'NONE', *, *, #51, .T. ) ;
#2750 = CARTESIAN_POINT ( 'NONE',  ( -2.782713018890638157, 5.315928322779165605, 5.504397606442132940 ) ) ;
#2751 = CARTESIAN_POINT ( 'NONE',  ( 4.435347140101024266, -4.403429997944519947, 11.36762589283694425 ) ) ;
#2752 = CARTESIAN_POINT ( 'NONE',  ( 0.9740856415301589744, -6.173834621338581741, 11.23852653055533857 ) ) ;
#2753 = CARTESIAN_POINT ( 'NONE',  ( -7.490007020835664164, -2.433650805992495503, 17.99999999999998934 ) ) ;
#2754 = CYLINDRICAL_SURFACE ( 'NONE', #4874, 0.9999999999999998890 ) ;
#2755 = CIRCLE ( 'NONE', #11641, 6.000000000000000888 ) ;
#2756 = FACE_BOUND ( 'NONE', #4547, .T. ) ;
#2757 = CARTESIAN_POINT ( 'NONE',  ( 1.035533905932739085, -2.500000000000000000, 1.949999999999999956 ) ) ;
#2758 = DIRECTION ( 'NONE',  ( -0.000000000000000000, 1.000000000000000000, -0.000000000000000000 ) ) ;
#2759 = SURFACE_STYLE_FILL_AREA ( #10313 ) ;
#2760 = DIRECTION ( 'NONE',  ( 0.9510565162951500895, 0.3090169943749582204, 0.000000000000000000 ) ) ;
#2761 = CARTESIAN_POINT ( 'NONE',  ( 2.500000000000000444, 184.7999999999999829, 7.000000000000000000 ) ) ;
#2762 = FACE_BOUND ( 'NONE', #11521, .T. ) ;
#2763 = CARTESIAN_POINT ( 'NONE',  ( -0.9962072163307928996, 227.6960174938032537, 5.361472040843871412 ) ) ;
#2764 = FACE_BOUND ( 'NONE', #5420, .T. ) ;
#2765 = CARTESIAN_POINT ( 'NONE',  ( 1.767766984964215471, 1.767766920968521616, -2.500000000000000444 ) ) ;
#2766 = CARTESIAN_POINT ( 'NONE',  ( -2.066987299999999639, 0.8561741729129455081, 1.200000001092474733 ) ) ;
#2767 = VECTOR ( 'NONE', #7880, 1000.000000000000000 ) ;
#2768 = CARTESIAN_POINT ( 'NONE',  ( 0.8561741729129456191, 188.3999999989075036, 4.933012699999999029 ) ) ;
#2769 = CARTESIAN_POINT ( 'NONE',  ( -2.692215568229928468, 5.362327947133553430, 18.26229037835931379 ) ) ;
#2770 = AXIS2_PLACEMENT_3D ( 'NONE', #176, #10049, #409 ) ;
#2772 = ORIENTED_EDGE ( 'NONE', *, *, #9307, .T. ) ;
#2771 = CARTESIAN_POINT ( 'NONE',  ( 2.066987299999999195, 189.1999999989075434, 7.856174172912946396 ) ) ;
#2773 = CARTESIAN_POINT ( 'NONE',  ( -4.291255145204092791, -4.544933371694659385, 17.38603820591928439 ) ) ;
#2774 = FACE_OUTER_BOUND ( 'NONE', #12641, .T. ) ;
#2775 = CARTESIAN_POINT ( 'NONE',  ( 0.000000000000000000, 187.2933328889893687, 9.583808270834989429 ) ) ;
#2776 = STYLED_ITEM ( 'NONE', ( #614 ), #15721 ) ;
#2777 = FACE_BOUND ( 'NONE', #103, .T. ) ;
#2778 = CARTESIAN_POINT ( 'NONE',  ( 2.746701853510111757, 189.9419816681355542, 6.030501831987404415 ) ) ;
#2779 = CARTESIAN_POINT ( 'NONE',  ( 0.004787046309016708585, -0.3999999999999975797, -2.483960639863540099 ) ) ;
#2780 = CARTESIAN_POINT ( 'NONE',  ( 2.997605338728016378, 189.8677746345552748, 7.530719179693556420 ) ) ;
#2781 = CARTESIAN_POINT ( 'NONE',  ( 6.143143148203054515, -1.154591847827728390, 5.613961794080713830 ) ) ;
#2782 = DIRECTION ( 'NONE',  ( -0.3090169943749447867, -0.9510565162951544194, 0.000000000000000000 ) ) ;
#2783 = CARTESIAN_POINT ( 'NONE',  ( 4.267558728637053100, 4.217879122113947332, 24.23617396794403334 ) ) ;
#2784 = EDGE_LOOP ( 'NONE', ( #6710, #2749, #1117, #11930 ) ) ;
#2785 = CARTESIAN_POINT ( 'NONE',  ( 2.066987300000000083, 186.0999999989075206, 6.143825827087054492 ) ) ;
#2786 = EDGE_CURVE ( 'NONE', #1897, #12110, #1948, .T. ) ;
#2787 = VERTEX_POINT ( 'NONE', #1748 ) ;
#2788 = CARTESIAN_POINT ( 'NONE',  ( 5.940390500375443139, 6.474944468551700361, 17.99999999999998934 ) ) ;
#2789 = MECHANICAL_DESIGN_GEOMETRIC_PRESENTATION_REPRESENTATION (  '', ( #4319 ), #14743 ) ;
#2790 = ORIENTED_EDGE ( 'NONE', *, *, #2740, .T. ) ;
#2791 = FACE_BOUND ( 'NONE', #14523, .T. ) ;
#2792 = CARTESIAN_POINT ( 'NONE',  ( -9.750000000000003553, 182.0000000000000000, -3.401296724241641415E-14 ) ) ;
#2793 = ORIENTED_EDGE ( 'NONE', *, *, #7772, .T. ) ;
#2794 = CARTESIAN_POINT ( 'NONE',  ( 1.461580736456472573, 1.461580736456472795, -2.249999998907525001 ) ) ;
#2795 = CARTESIAN_POINT ( 'NONE',  ( -2.817313151351189315, 5.579000502529432026, 4.867658743658316745 ) ) ;
#2796 = CARTESIAN_POINT ( 'NONE',  ( -1.514810195292803918, 190.0478454264466848, 4.614282054999431004 ) ) ;
#2797 = DIRECTION ( 'NONE',  ( 0.000000000000000000, -2.775557561562887900E-16, 1.000000000000000000 ) ) ;
#2798 = CARTESIAN_POINT ( 'NONE',  ( 2.500000000000000444, -1.035533905932737309, -0.3500000000000000333 ) ) ;
#2799 = CARTESIAN_POINT ( 'NONE',  ( -3.420311045507932857, 4.931422832349230845, 16.99992038825522656 ) ) ;
#2800 = CONTEXT_DEPENDENT_SHAPE_REPRESENTATION ( #8339, #9592 ) ;
#2801 = AXIS2_PLACEMENT_3D ( 'NONE', #11095, #9832, #14682 ) ;
#2802 = CARTESIAN_POINT ( 'NONE',  ( 4.286401442266532413, 4.198423832313196158, 5.000000000000004441 ) ) ;
#2803 = CARTESIAN_POINT ( 'NONE',  ( -0.8561741729129455081, 2.066987299999999639, -0.2999999989075253226 ) ) ;
#2804 = CARTESIAN_POINT ( 'NONE',  ( -6.021167129161077547, 1.680051667990220432, 30.02640428276698259 ) ) ;
#2805 = CARTESIAN_POINT ( 'NONE',  ( -0.09789622041826565035, 228.2551366570249343, 10.16828389758070550 ) ) ;
#2806 = B_SPLINE_CURVE_WITH_KNOTS ( 'NONE', 3,
 ( #3933, #11338, #8892, #10230, #9919, #5145, #1703, #2909, #13637, #13874, #2752, #6505, #2986, #4177, #7759, #12686, #14772, #7603 ),
 .UNSPECIFIED., .F., .F.,
 ( 4, 2, 2, 2, 2, 2, 2, 2, 4 ),
 ( 0.000000000000000000, 0.0003914362731607611522, 0.0007828725463215223043, 0.001174308819482283456, 0.001565745092643044609, 0.001957181365803805761, 0.002348617638964566913, 0.002740053912125328065, 0.003131490185286089217 ),
 .UNSPECIFIED. ) ;
#2807 = EDGE_CURVE ( 'NONE', #5516, #5575, #15389, .T. ) ;
#2808 = VERTEX_POINT ( 'NONE', #11530 ) ;
#2809 = EDGE_LOOP ( 'NONE', ( #15512, #3317, #2949, #4891 ) ) ;
#2810 = EDGE_LOOP ( 'NONE', ( #11313, #12814, #9995, #6948 ) ) ;
#2811 = ORIENTED_EDGE ( 'NONE', *, *, #4181, .F. ) ;
#2812 = CARTESIAN_POINT ( 'NONE',  ( 0.000000000000000000, 2.000000000000000000, 0.000000000000000000 ) ) ;
#2813 = VERTEX_POINT ( 'NONE', #5350 ) ;
#2814 = FACE_OUTER_BOUND ( 'NONE', #11179, .T. ) ;
#2815 = CARTESIAN_POINT ( 'NONE',  ( -4.006441409774754270, -4.467329318258197901, 18.79888242247939800 ) ) ;
#2816 = CARTESIAN_POINT ( 'NONE',  ( -0.6151877315909333177, 6.220340188096021627, 18.79906673469662337 ) ) ;
#2817 = CARTESIAN_POINT ( 'NONE',  ( 5.571002711501426674, -2.833546409886251283, 30.73620383159192571 ) ) ;
#2818 = CARTESIAN_POINT ( 'NONE',  ( -1.035533905932737753, 185.7499999978150527, 4.500000000000000888 ) ) ;
#2819 = CARTESIAN_POINT ( 'NONE',  ( -6.176542424588110869, 0.9554180641286129649, 11.49999999999998224 ) ) ;
#2820 = CARTESIAN_POINT ( 'NONE',  ( -4.290821322214440237, 4.545321419741492619, 10.88558052754513383 ) ) ;
#2821 = EDGE_CURVE ( 'NONE', #10136, #13172, #8945, .T. ) ;
#2822 = CARTESIAN_POINT ( 'NONE',  ( 3.419318284370178596, 4.932111238568190892, 10.50007997643736424 ) ) ;
#2823 = CARTESIAN_POINT ( 'NONE',  ( -1.361387964035781121E-13, 106.0000000000000142, 9.750000000000003553 ) ) ;
#2824 = CARTESIAN_POINT ( 'NONE',  ( 2.500000000000000444, 187.1699999975965625, 7.000000000000000000 ) ) ;
#2825 = CARTESIAN_POINT ( 'NONE',  ( -0.3256308520141213414, 228.9034500205340237, 8.848606045481535176 ) ) ;
#2826 = CARTESIAN_POINT ( 'NONE',  ( -2.990426535912302786, 227.3682058476787233, 7.559219386994686651 ) ) ;
#2827 = B_SPLINE_CURVE_WITH_KNOTS ( 'NONE', 3,
 ( #13316, #2657, #1377, #7511, #3842, #6251, #13474, #12278, #3609, #1297, #7588, #11243, #2576, #14758, #111, #12355, #11167, #13548 ),
 .UNSPECIFIED., .F., .F.,
 ( 4, 2, 2, 2, 2, 2, 2, 2, 4 ),
 ( 0.003131923598876996170, 0.003523316383094313078, 0.003914709167311630419, 0.004306101951528947328, 0.004697494735746264236, 0.005088887519963581144, 0.005480280304180898052, 0.005871673088398214960, 0.006263065872615531868 ),
 .UNSPECIFIED. ) ;
#2828 = CARTESIAN_POINT ( 'NONE',  ( -0.9975586949907861989, 189.0634563462267010, 10.01833148473745894 ) ) ;
#2829 = EDGE_CURVE ( 'NONE', #10051, #13722, #2476, .T. ) ;
#2830 = VERTEX_POINT ( 'NONE', #8278 ) ;
#2831 = CARTESIAN_POINT ( 'NONE',  ( -4.267992336621191818, 4.217442018460005215, 5.261943240031468960 ) ) ;
#2832 = DIRECTION ( 'NONE',  ( 0.000000000000000000, 0.000000000000000000, 1.000000000000000000 ) ) ;
#2833 = CARTESIAN_POINT ( 'NONE',  ( -3.107583187530600810, 5.133966411712579614, 23.62619317285289000 ) ) ;
#2834 = CARTESIAN_POINT ( 'NONE',  ( 6.143020266950977692, 1.155160780047711944, 12.11441947245482353 ) ) ;
#2835 = DIRECTION ( 'NONE',  ( -0.5877852522924685852, -0.8090169943749508930, 0.000000000000000000 ) ) ;
#2836 = EDGE_CURVE ( 'NONE', #15371, #8616, #14150, .T. ) ;
#2837 = CARTESIAN_POINT ( 'NONE',  ( -2.931212650151596932, -5.520239928492851611, 31.50425949503010514 ) ) ;
#2838 = VECTOR ( 'NONE', #5540, 1000.000000000000114 ) ;
#2839 = CARTESIAN_POINT ( 'NONE',  ( -1.530808498934191571E-16, 2.500000000000000000, 2.299999999999999822 ) ) ;
#2840 = CARTESIAN_POINT ( 'NONE',  ( 1.767766952966368432, 188.7000000000000171, 8.767766952966368876 ) ) ;
#2841 =( LENGTH_UNIT ( ) NAMED_UNIT ( * ) SI_UNIT ( .MILLI., .METRE. ) );
#2842 = CYLINDRICAL_SURFACE ( 'NONE', #13854, 1.000000000000000666 ) ;
#2843 = CARTESIAN_POINT ( 'NONE',  ( -5.421010862427522170E-17, 187.4000000000000057, 4.500000000000000000 ) ) ;
#2844 = FACE_BOUND ( 'NONE', #12793, .T. ) ;
#2845 = CARTESIAN_POINT ( 'NONE',  ( 1.314367061980813878, 227.7707019980692564, 5.577165148888615143 ) ) ;
#2846 = CARTESIAN_POINT ( 'NONE',  ( -1.265664690411614835E-16, 2.066987299999999639, -1.949999998907525622 ) ) ;
#2847 = CARTESIAN_POINT ( 'NONE',  ( -2.931156713028435501, -5.520271803279239720, 10.99563030319846746 ) ) ;
#2848 = CARTESIAN_POINT ( 'NONE',  ( 0.000000000000000000, -0.001000000000000132727, -11.50000000000000000 ) ) ;
#2849 = CARTESIAN_POINT ( 'NONE',  ( -1.461580736456473906, 187.9499999989075150, 8.461580736456474128 ) ) ;
#2850 = LINE ( 'NONE', #5244, #10363 ) ;
#2852 = ORIENTED_EDGE ( 'NONE', *, *, #11933, .T. ) ;
#2851 = CARTESIAN_POINT ( 'NONE',  ( 0.8561741729129455081, 186.9999999989075263, 4.933012699999999029 ) ) ;
#2853 = DIRECTION ( 'NONE',  ( 0.000000000000000000, 1.000000000000000000, 0.000000000000000000 ) ) ;
#2854 = DIRECTION ( 'NONE',  ( 0.8090169943749510040, -0.5877852522924683631, 0.000000000000000000 ) ) ;
#2855 = CARTESIAN_POINT ( 'NONE',  ( -5.931817299736865223, 0.9033986943601339803, 4.737709621640688873 ) ) ;
#2856 = CARTESIAN_POINT ( 'NONE',  ( 2.265240160886509813, 189.1526725940605331, 9.149827916924719418 ) ) ;
#2857 = CARTESIAN_POINT ( 'NONE',  ( 0.0001777891039407533040, -0.3999999999999906408, -2.457936153810343693 ) ) ;
#2858 =( BOUNDED_CURVE ( )  B_SPLINE_CURVE ( 2, ( #12059, #4751, #13488, #2591, #1390, #9770, #15572, #8581, #1084 ),
 .UNSPECIFIED., .F., .F. ) 
 B_SPLINE_CURVE_WITH_KNOTS ( ( 3, 2, 2, 2, 3 ),
 ( 0.5714285714285713969, 0.5892857142857143016, 0.6071428571428570953, 0.6250000000000000000, 0.6428571428571429047 ),
 .UNSPECIFIED. ) 
 CURVE ( )  GEOMETRIC_REPRESENTATION_ITEM ( )  RATIONAL_B_SPLINE_CURVE ( ( 1.000000000000000000, 0.9238795325112867385, 1.000000000000000000, 0.9238795325112867385, 1.000000000000000000, 0.9238795325112867385, 1.000000000000000000, 0.9238795325112867385, 1.000000000000000000 ) ) 
 REPRESENTATION_ITEM ( '' )  );
#2859 = CARTESIAN_POINT ( 'NONE',  ( 2.985698417011507733, 189.8946583874339638, 6.934546546956198654 ) ) ;
#2860 = CARTESIAN_POINT ( 'NONE',  ( -2.849573632035271586, 5.280958870664604454, 30.38438267301394902 ) ) ;
#2861 = FACE_OUTER_BOUND ( 'NONE', #11217, .T. ) ;
#2862 = CARTESIAN_POINT ( 'NONE',  ( -5.915641100987811818, -1.003868594704857342, 10.99571079637978599 ) ) ;
#2863 = ORIENTED_EDGE ( 'NONE', *, *, #7405, .T. ) ;
#2864 = CARTESIAN_POINT ( 'NONE',  ( -2.066987300000000083, 185.6499999989075320, 7.000000000000000000 ) ) ;
#2865 = ORIENTED_EDGE ( 'NONE', *, *, #13918, .T. ) ;
#2866 = CARTESIAN_POINT ( 'NONE',  ( -5.317509234263837037, -2.779225709351230922, 24.36938304467860306 ) ) ;
#2867 = ORIENTED_EDGE ( 'NONE', *, *, #7594, .T. ) ;
#2868 = VECTOR ( 'NONE', #1926, 1000.000000000000114 ) ;
#2869 = CARTESIAN_POINT ( 'NONE',  ( 7.799024015210672900, -1.482594289696959944, 17.99999999999998934 ) ) ;
#2870 = CARTESIAN_POINT ( 'NONE',  ( 7.490007020835748541, -2.433650805992050969, 24.49999999999999289 ) ) ;
#2871 = ORIENTED_EDGE ( 'NONE', *, *, #6631, .T. ) ;
#2872 = CARTESIAN_POINT ( 'NONE',  ( 0.8561741729129463963, -2.066987299999999195, -0.09999999890752520049 ) ) ;
#2873 = CARTESIAN_POINT ( 'NONE',  ( -4.416678568553696671, 4.422441866694263979, 4.737630265561251441 ) ) ;
#2874 = CARTESIAN_POINT ( 'NONE',  ( -2.900132499248337936, 189.9172581111519094, 6.475756817537924093 ) ) ;
#2875 = CARTESIAN_POINT ( 'NONE',  ( 0.8561741729129457301, 189.0999999989075206, 9.066987299999999195 ) ) ;
#2876 = CARTESIAN_POINT ( 'NONE',  ( -2.500000000000000444, 1.035533905932737753, -1.549999999999999600 ) ) ;
#2877 = EDGE_CURVE ( 'NONE', #13893, #6615, #5812, .T. ) ;
#2878 = CARTESIAN_POINT ( 'NONE',  ( 2.500000000000000000, 3.061616997868383141E-16, -1.100000000000000311 ) ) ;
#2879 = CARTESIAN_POINT ( 'NONE',  ( -4.286401442266688733, 4.198423832313033621, 17.99999999999998934 ) ) ;
#2880 = DIRECTION ( 'NONE',  ( 0.000000000000000000, 0.000000000000000000, 1.000000000000000000 ) ) ;
#2881 = CARTESIAN_POINT ( 'NONE',  ( 2.066987299999999639, 2.531329380823229670E-16, 0.2500000010924748328 ) ) ;
#2882 = CARTESIAN_POINT ( 'NONE',  ( -0.8736772044959679739, 6.188841968496064716, 30.49611573292809652 ) ) ;
#2883 = ORIENTED_EDGE ( 'NONE', *, *, #3113, .T. ) ;
#2884 = ORIENTED_EDGE ( 'NONE', *, *, #6115, .T. ) ;
#2885 = ORIENTED_EDGE ( 'NONE', *, *, #13327, .F. ) ;
#2886 = CARTESIAN_POINT ( 'NONE',  ( 0.8738118504727017122, 5.936246475285011925, 18.50357242174242245 ) ) ;
#2887 = CARTESIAN_POINT ( 'NONE',  ( 5.649053410273043418, 2.675685104943323012, 4.384822196241565884 ) ) ;
#2888 = ORIENTED_EDGE ( 'NONE', *, *, #11475, .T. ) ;
#2889 = CARTESIAN_POINT ( 'NONE',  ( -6.172552660730961094, -0.9821660343539843074, 17.73620383159192926 ) ) ;
#2890 = CIRCLE ( 'NONE', #12790, 6.250000000000000888 ) ;
#2891 = CARTESIAN_POINT ( 'NONE',  ( 0.5039005892422661059, -6.230833003620530164, 17.12636388911296592 ) ) ;
#2892 = EDGE_CURVE ( 'NONE', #7816, #5247, #6563, .T. ) ;
#2893 = CARTESIAN_POINT ( 'NONE',  ( -0.1306394121197964608, 6.250000000000004441, 16.99999999999998934 ) ) ;
#2894 = CARTESIAN_POINT ( 'NONE',  ( 0.2023276174864365173, -0.3999999999999906408, -2.561683098400944658 ) ) ;
#2895 = FACE_OUTER_BOUND ( 'NONE', #7060, .T. ) ;
#2896 = CARTESIAN_POINT ( 'NONE',  ( 2.500000000000000444, 1.035533905932737975, 2.156999999978150395 ) ) ;
#2897 = EDGE_CURVE ( 'NONE', #860, #15705, #2270, .T. ) ;
#2898 = FACE_OUTER_BOUND ( 'NONE', #13292, .T. ) ;
#2899 = DIRECTION ( 'NONE',  ( 0.000000000000000000, 0.000000000000000000, 1.000000000000000000 ) ) ;
#2900 = CARTESIAN_POINT ( 'NONE',  ( 1.035533905932738197, 187.8199999975965682, 9.500000000000003553 ) ) ;
#2901 = CARTESIAN_POINT ( 'NONE',  ( 1.625192428541204714, 228.1012562471100011, 9.715842694323066908 ) ) ;
#2902 = CARTESIAN_POINT ( 'NONE',  ( -0.9651034952757481244, 226.3762748196293728, 4.637298184581183591 ) ) ;
#2903 = EDGE_LOOP ( 'NONE', ( #10669, #10071, #6382, #15255, #14376, #9527, #573, #9579, #11775, #14567, #8966, #5482, #1270, #11705, #7075 ) ) ;
#2904 = CARTESIAN_POINT ( 'NONE',  ( -2.500000000000000000, 0.000000000000000000, 0.2000000021849497878 ) ) ;
#2905 = ORIENTED_EDGE ( 'NONE', *, *, #12295, .T. ) ;
#2906 = DIRECTION ( 'NONE',  ( 1.000000000000000000, 0.000000000000000000, 0.000000000000000000 ) ) ;
#2907 = CIRCLE ( 'NONE', #4951, 5.000000000000000000 ) ;
#2908 = CARTESIAN_POINT ( 'NONE',  ( 0.000000000000000000, 184.0000000000000000, -7.000000000000000000 ) ) ;
#2909 = CARTESIAN_POINT ( 'NONE',  ( 0.9735954530125885409, -6.173909381473981384, 11.76281793585243918 ) ) ;
#2910 = CARTESIAN_POINT ( 'NONE',  ( 5.558508435838221295, 2.857531096718871844, 11.49999999999998224 ) ) ;
#2911 = CARTESIAN_POINT ( 'NONE',  ( 0.000000000000000000, 0.000000000000000000, -2.500000000000000000 ) ) ;
#2912 = CARTESIAN_POINT ( 'NONE',  ( 3.632753594129220165, -4.777047695051066967, 23.50004946353777413 ) ) ;
#2913 = CARTESIAN_POINT ( 'NONE',  ( -1.035533905932738197, -2.500000000000000000, 1.849999999999999867 ) ) ;
#2914 = CARTESIAN_POINT ( 'NONE',  ( 4.286401442266532413, 4.198423832313196158, 5.000000000000004441 ) ) ;
#2915 =( NAMED_UNIT ( * ) PLANE_ANGLE_UNIT ( ) SI_UNIT ( $, .RADIAN. ) );
#2916 = EDGE_CURVE ( 'NONE', #4415, #8748, #15279, .T. ) ;
#2917 = CARTESIAN_POINT ( 'NONE',  ( 5.903230462362944131, 1.077253041748938989, 5.614425215719392348 ) ) ;
#2918 = CARTESIAN_POINT ( 'NONE',  ( 1.035533905932737975, 185.7500000000000568, 4.500000000000000888 ) ) ;
#2919 = VECTOR ( 'NONE', #8245, 1000.000000000000000 ) ;
#2920 = CARTESIAN_POINT ( 'NONE',  ( -1.864073305829632599, 228.0308260764439297, 6.328418323741104246 ) ) ;
#2921 = DIRECTION ( 'NONE',  ( -1.000000000000000000, 0.000000000000000000, 0.000000000000000000 ) ) ;
#2922 = CARTESIAN_POINT ( 'NONE',  ( 5.858736126997225568, -2.179962889276819027, 25.47359571723300675 ) ) ;
#2923 =( REPRESENTATION_RELATIONSHIP ('NONE','NONE', #11191, #3660 ) REPRESENTATION_RELATIONSHIP_WITH_TRANSFORMATION ( #6955 )SHAPE_REPRESENTATION_RELATIONSHIP( ) );
#2924 = CARTESIAN_POINT ( 'NONE',  ( 2.066987299999999639, 2.531329380823229670E-16, 1.650000001092474911 ) ) ;
#2925 = EDGE_CURVE ( 'NONE', #3329, #5268, #5890, .T. ) ;
#2926 = CARTESIAN_POINT ( 'NONE',  ( 1.461580736456473240, 188.3499999989074922, 5.538419263543526760 ) ) ;
#2927 = CARTESIAN_POINT ( 'NONE',  ( -5.931817299736830584, -0.9033986943603558029, 18.26229037835932090 ) ) ;
#2929 = VERTEX_POINT ( 'NONE', #1026 ) ;
#2928 = CARTESIAN_POINT ( 'NONE',  ( -1.461580736456473462, 187.3499999989075206, 8.461580736456472351 ) ) ;
#2930 = CARTESIAN_POINT ( 'NONE',  ( -2.997451966578457139, -5.485105005465983119, 17.38482219624156855 ) ) ;
#2931 =( GEOMETRIC_REPRESENTATION_CONTEXT ( 3 ) GLOBAL_UNCERTAINTY_ASSIGNED_CONTEXT ( ( #13315 ) ) GLOBAL_UNIT_ASSIGNED_CONTEXT ( ( #7998, #8752, #2695 ) ) REPRESENTATION_CONTEXT ( 'NONE', 'WORKASPACE' ) );
#2932 = CARTESIAN_POINT ( 'NONE',  ( 6.081590040723096280, -1.446205118472926099, 12.37367328635990837 ) ) ;
#2933 = CARTESIAN_POINT ( 'NONE',  ( -0.001074311305641557088, 226.3251817249170017, 4.486671161788877704 ) ) ;
#2934 = SURFACE_STYLE_FILL_AREA ( #15029 ) ;
#2935 = ADVANCED_FACE ( 'NONE', ( #14071 ), #2057, .F. ) ;
#2936 = CARTESIAN_POINT ( 'NONE',  ( 2.927574602831448658, 189.9114408209157148, 6.589606913355709139 ) ) ;
#2937 = DIRECTION ( 'NONE',  ( -0.5877852522924685852, -0.8090169943749507819, 0.000000000000000000 ) ) ;
#2938 = CARTESIAN_POINT ( 'NONE',  ( -0.8737888311109888173, 5.936248257219512325, 31.50344185141217679 ) ) ;
#2939 = CARTESIAN_POINT ( 'NONE',  ( 2.917903144078069833, 189.9135866353617814, 6.547191606018472498 ) ) ;
#2940 = CARTESIAN_POINT ( 'NONE',  ( 6.155912734541134412, -1.081577393120893182, 5.503892131249681796 ) ) ;
#2941 = DIRECTION ( 'NONE',  ( 0.000000000000000000, 0.000000000000000000, 1.000000000000000000 ) ) ;
#2942 = DIRECTION ( 'NONE',  ( -1.062480551894329468E-17, -3.608224830031754812E-16, 1.000000000000000000 ) ) ;
#2943 = VERTEX_POINT ( 'NONE', #866 ) ;
#2944 = CARTESIAN_POINT ( 'NONE',  ( -4.946672411965113980E-16, 185.8499999989075206, 9.066987300000000971 ) ) ;
#2945 = ORIENTED_EDGE ( 'NONE', *, *, #4680, .F. ) ;
#2946 = DIRECTION ( 'NONE',  ( 1.000000000000000000, 0.000000000000000000, 0.000000000000000000 ) ) ;
#2947 = VERTEX_POINT ( 'NONE', #7005 ) ;
#2948 = FACE_OUTER_BOUND ( 'NONE', #13927, .T. ) ;
#2949 = ORIENTED_EDGE ( 'NONE', *, *, #12636, .T. ) ;
#2950 = CARTESIAN_POINT ( 'NONE',  ( -2.668367453516630849, -5.373994336898131330, 5.132360785839114925 ) ) ;
#2951 =( BOUNDED_CURVE ( )  B_SPLINE_CURVE ( 2, ( #813, #4638, #12904, #9411, #9332, #14174, #5756, #11636, #8063 ),
 .UNSPECIFIED., .F., .F. ) 
 B_SPLINE_CURVE_WITH_KNOTS ( ( 3, 2, 2, 2, 3 ),
 ( 0.1428571428571428492, 0.1607142857142857262, 0.1785714285714285754, 0.1964285714285714246, 0.2142857142857142738 ),
 .UNSPECIFIED. ) 
 CURVE ( )  GEOMETRIC_REPRESENTATION_ITEM ( )  RATIONAL_B_SPLINE_CURVE ( ( 1.000000000000000000, 0.9238795325112867385, 1.000000000000000000, 0.9238795325112867385, 1.000000000000000000, 0.9238795325112867385, 1.000000000000000000, 0.9238795325112867385, 1.000000000000000000 ) ) 
 REPRESENTATION_ITEM ( '' )  );
#2952 = AXIS2_PLACEMENT_3D ( 'NONE', #2550, #14647, #10822 ) ;
#2953 = CARTESIAN_POINT ( 'NONE',  ( -2.931212650151651555, 5.520239928492821413, 4.495740504969916174 ) ) ;
#2954 = CARTESIAN_POINT ( 'NONE',  ( 3.118365096457673680, 189.0000000000000000, 7.000000000000000000 ) ) ;
#2955 = CARTESIAN_POINT ( 'NONE',  ( -1.767766952966369098, 1.767766952966369098, 1.700000002184949732 ) ) ;
#2956 = CARTESIAN_POINT ( 'NONE',  ( 2.000000000000001776, -4.331536797758218293E-16, 2.750000000000002665 ) ) ;
#2957 = CYLINDRICAL_SURFACE ( 'NONE', #1104, 0.9999999999999998890 ) ;
#2958 = CARTESIAN_POINT ( 'NONE',  ( -5.615973259022225328, -2.743340227996369673, 25.00389213124970311 ) ) ;
#2959 = CARTESIAN_POINT ( 'NONE',  ( -2.066987299999999639, 0.000000000000000000, -1.749999998907525223 ) ) ;
#2960 = CARTESIAN_POINT ( 'NONE',  ( 2.668367453516568677, 5.373994336898162416, 11.49999999999998224 ) ) ;
#2961 = ORIENTED_EDGE ( 'NONE', *, *, #1355, .T. ) ;
#2962 = ORIENTED_EDGE ( 'NONE', *, *, #4651, .F. ) ;
#2963 = AXIS2_PLACEMENT_3D ( 'NONE', #12714, #3017, #3324 ) ;
#2964 = ORIENTED_EDGE ( 'NONE', *, *, #11635, .T. ) ;
#2965 = CARTESIAN_POINT ( 'NONE',  ( 4.069800786343793497, -4.744882212776830421, 12.37381964045070681 ) ) ;
#2966 = LINE ( 'NONE', #1683, #10890 ) ;
#2967 = ORIENTED_EDGE ( 'NONE', *, *, #3402, .F. ) ;
#2968 = DIRECTION ( 'NONE',  ( 0.000000000000000000, 0.000000000000000000, 1.000000000000000000 ) ) ;
#2969 = CARTESIAN_POINT ( 'NONE',  ( -1.767766952966369098, 1.767766952966369098, 1.700000002184949510 ) ) ;
#2970 = CARTESIAN_POINT ( 'NONE',  ( -5.842988226680587260, 1.369004370660612313, 5.873806827147107334 ) ) ;
#2971 = CARTESIAN_POINT ( 'NONE',  ( 0.1306070469494795272, 6.249999999999999112, 16.99999999999998579 ) ) ;
#2972 = CARTESIAN_POINT ( 'NONE',  ( -1.035533905932739529, 185.2499999978150811, 9.500000000000003553 ) ) ;
#2973 = DIRECTION ( 'NONE',  ( 0.8090169943749421222, 0.5877852522924802425, 0.000000000000000000 ) ) ;
#2974 = DIRECTION ( 'NONE',  ( 0.000000000000000000, 0.000000000000000000, 1.000000000000000000 ) ) ;
#2975 = DIRECTION ( 'NONE',  ( 0.000000000000000000, 0.000000000000000000, 1.000000000000000000 ) ) ;
#2976 = CARTESIAN_POINT ( 'NONE',  ( -1.767766952966369098, 185.0699999975965397, 5.232233047033630235 ) ) ;
#2977 = CARTESIAN_POINT ( 'NONE',  ( -1.619108980504621043, 228.6400225536183655, 8.087812496111112637 ) ) ;
#2978 = CARTESIAN_POINT ( 'NONE',  ( -2.439580969806472321, 226.7272467340407331, 5.671663139905907869 ) ) ;
#2979 =( BOUNDED_CURVE ( )  B_SPLINE_CURVE ( 2, ( #8358, #9308, #14146, #6929, #4376, #11762, #10652, #1023, #864 ),
 .UNSPECIFIED., .F., .F. ) 
 B_SPLINE_CURVE_WITH_KNOTS ( ( 3, 2, 2, 2, 3 ),
 ( 0.3571428571428571508, 0.3750000000000000000, 0.3928571428571428492, 0.4107142857142856984, 0.4285714285714285476 ),
 .UNSPECIFIED. ) 
 CURVE ( )  GEOMETRIC_REPRESENTATION_ITEM ( )  RATIONAL_B_SPLINE_CURVE ( ( 1.000000000000000000, 0.9238795325112867385, 1.000000000000000000, 0.9238795325112867385, 1.000000000000000000, 0.9238795325112867385, 1.000000000000000000, 0.9238795325112867385, 1.000000000000000000 ) ) 
 REPRESENTATION_ITEM ( '' )  );
#2980 = ORIENTED_EDGE ( 'NONE', *, *, #5079, .F. ) ;
#2981 = EDGE_CURVE ( 'NONE', #15355, #159, #8173, .T. ) ;
#2982 = CARTESIAN_POINT ( 'NONE',  ( 2.500000000000000000, 3.061616997868383141E-16, 0.6000000021849497545 ) ) ;
#2983 = EDGE_LOOP ( 'NONE', ( #8310, #11623 ) ) ;
#2984 = EDGE_CURVE ( 'NONE', #9629, #13232, #9852, .T. ) ;
#2985 = CARTESIAN_POINT ( 'NONE',  ( -4.435347140101170815, 4.403429997944374286, 17.86939309276499799 ) ) ;
#2986 = CARTESIAN_POINT ( 'NONE',  ( 0.8002720181891768148, -6.199262377003395663, 10.88606262465556895 ) ) ;
#2987 = CARTESIAN_POINT ( 'NONE',  ( 0.000000000000000000, 0.000000000000000000, 0.000000000000000000 ) ) ;
#2988 = DIRECTION ( 'NONE',  ( 0.8090169943749506709, -0.5877852522924686962, 0.000000000000000000 ) ) ;
#2989 = ADVANCED_FACE ( 'NONE', ( #12004 ), #11129, .F. ) ;
#2990 = LINE ( 'NONE', #11185, #15292 ) ;
#2991 = CARTESIAN_POINT ( 'NONE',  ( 2.500000000000000444, -1.035533905932737309, 2.050000000000000266 ) ) ;
#2992 = CARTESIAN_POINT ( 'NONE',  ( -1.035533905932737753, 2.500000000000000444, -0.05000000000000014155 ) ) ;
#2993 = DIRECTION ( 'NONE',  ( -6.123233995736766036E-17, 1.000000000000000000, 0.000000000000000000 ) ) ;
#2994 =( GEOMETRIC_REPRESENTATION_CONTEXT ( 3 ) GLOBAL_UNCERTAINTY_ASSIGNED_CONTEXT ( ( #6009 ) ) GLOBAL_UNIT_ASSIGNED_CONTEXT ( ( #6118, #10880, #9860 ) ) REPRESENTATION_CONTEXT ( 'NONE', 'WORKASPACE' ) );
#2995 = CARTESIAN_POINT ( 'NONE',  ( 0.8499999999999896527, -0.3999999999999958589, 2.619018321873339161 ) ) ;
#2996 = CARTESIAN_POINT ( 'NONE',  ( 2.500000000000000444, 187.1499999999999773, 8.035533905932739529 ) ) ;
#2997 = CARTESIAN_POINT ( 'NONE',  ( -0.1316767729515891938, 227.6100531710845587, 5.113202173749356483 ) ) ;
#2998 = CARTESIAN_POINT ( 'NONE',  ( 6.106056299406778187, -1.336851112280531995, 17.20112161576660981 ) ) ;
#2999 = CARTESIAN_POINT ( 'NONE',  ( 0.09128442572522987852, 0.4000000000000062395, -2.551849451881606168 ) ) ;
#3000 = ADVANCED_FACE ( 'NONE', ( #1199 ), #10815, .F. ) ;
#3001 = CARTESIAN_POINT ( 'NONE',  ( -2.066987299999999639, 0.8561741729129455081, -0.3999999989075251339 ) ) ;
#3002 = CARTESIAN_POINT ( 'NONE',  ( 1.035533905932738419, 185.4499999999999886, 9.500000000000003553 ) ) ;
#3003 = CARTESIAN_POINT ( 'NONE',  ( -1.035533905932737975, 187.3499999978151038, 4.500000000000001776 ) ) ;
#3004 = AXIS2_PLACEMENT_3D ( 'NONE', #12157, #11913, #65 ) ;
#3006 = ORIENTED_EDGE ( 'NONE', *, *, #14994, .T. ) ;
#3005 = CARTESIAN_POINT ( 'NONE',  ( -2.066987300000000083, 187.2499999989075263, 7.000000000000000000 ) ) ;
#3007 = LINE ( 'NONE', #14944, #3307 ) ;
#3008 = CARTESIAN_POINT ( 'NONE',  ( 3.107278289587024567, 5.134157760522150227, 25.37364704684422279 ) ) ;
#3009 = CARTESIAN_POINT ( 'NONE',  ( 3.659182332138073087E-16, 190.0875178197511275, 4.201689379953569947 ) ) ;
#3010 = FACE_OUTER_BOUND ( 'NONE', #11955, .T. ) ;
#3011 = CARTESIAN_POINT ( 'NONE',  ( 2.763434297034058407, 189.2181571714553741, 8.347543543386905185 ) ) ;
#3012 = LINE ( 'NONE', #5488, #456 ) ;
#3013 = CARTESIAN_POINT ( 'NONE',  ( -5.317509234263930296, -2.779225709351048401, 5.000000000000004441 ) ) ;
#3014 = CARTESIAN_POINT ( 'NONE',  ( 0.2786071629746884604, 190.0868662572826793, 4.208169715142605405 ) ) ;
#3016 = CARTESIAN_POINT ( 'NONE',  ( 6.143020266951017661, -1.155160780047501445, 23.88558052754514804 ) ) ;
#3015 = AXIS2_PLACEMENT_3D ( 'NONE', #13723, #13797, #8655 ) ;
#3017 = DIRECTION ( 'NONE',  ( 0.000000000000000000, 0.000000000000000000, 1.000000000000000000 ) ) ;
#3018 = LINE ( 'NONE', #12481, #15604 ) ;
#3019 = EDGE_LOOP ( 'NONE', ( #10341, #3265 ) ) ;
#3020 = CARTESIAN_POINT ( 'NONE',  ( -2.066987300000000527, 186.2499999989074979, 7.000000000000000000 ) ) ;
#3021 = ORIENTED_EDGE ( 'NONE', *, *, #8094, .F. ) ;
#3022 = CARTESIAN_POINT ( 'NONE',  ( -5.903057025253887424, 1.078199533779612640, 25.11561732698604388 ) ) ;
#3023 = ORIENTED_EDGE ( 'NONE', *, *, #13034, .F. ) ;
#3024 = ADVANCED_FACE ( 'NONE', ( #3492 ), #8680, .F. ) ;
#3025 = FACE_OUTER_BOUND ( 'NONE', #12229, .T. ) ;
#3026 = DIRECTION ( 'NONE',  ( -0.9510565162951545304, 0.3090169943749447867, 0.000000000000000000 ) ) ;
#3027 = AXIS2_PLACEMENT_3D ( 'NONE', #14925, #4016, #6506 ) ;
#3028 = PRODUCT_DEFINITION ( 'UNKNOWN', '', #12132, #10242 ) ;
#3029 = CARTESIAN_POINT ( 'NONE',  ( -4.196288036172359348, -4.288789315524921264, 5.503120489023787698 ) ) ;
#3030 = CARTESIAN_POINT ( 'NONE',  ( 0.8730424326980882332, 5.936362132114464174, 4.495006902185632036 ) ) ;
#3031 = LINE ( 'NONE', #7961, #6429 ) ;
#3032 = CARTESIAN_POINT ( 'NONE',  ( 1.035533905932737531, 2.500000000000000444, -0.1499999999999999667 ) ) ;
#3033 = CARTESIAN_POINT ( 'NONE',  ( -3.061616997868391523E-16, 182.0000000000000000, 7.000000000000000000 ) ) ;
#3034 = CARTESIAN_POINT ( 'NONE',  ( -3.107583187530535529, 5.133966411712619582, 17.12619317285288645 ) ) ;
#3035 = DIRECTION ( 'NONE',  ( -0.3090169943749446202, -0.9510565162951544194, 0.000000000000000000 ) ) ;
#3036 = CARTESIAN_POINT ( 'NONE',  ( 3.568242062701521444, 5.132954954975510908, 32.00004906876532829 ) ) ;
#3037 = CARTESIAN_POINT ( 'NONE',  ( 2.692143549875342767, 5.362363179736505003, 11.76194324003145830 ) ) ;
#3038 = VERTEX_POINT ( 'NONE', #14553 ) ;
#3039 = AXIS2_PLACEMENT_3D ( 'NONE', #6856, #13626, #10063 ) ;
#3040 = ORIENTED_EDGE ( 'NONE', *, *, #15555, .F. ) ;
#3041 = VERTEX_POINT ( 'NONE', #3649 ) ;
#3042 = CARTESIAN_POINT ( 'NONE',  ( 2.841163418881408553, -5.567120626447921161, 11.76236973443872280 ) ) ;
#3043 = CARTESIAN_POINT ( 'NONE',  ( 5.558508435838189321, 2.857531096718932240, 5.000000000000004441 ) ) ;
#3044 = ORIENTED_EDGE ( 'NONE', *, *, #9648, .F. ) ;
#3045 = CARTESIAN_POINT ( 'NONE',  ( 5.665824935993658329, -1.978765057080782652, 18.99995053646221521 ) ) ;
#3046 = B_SPLINE_CURVE_WITH_KNOTS ( 'NONE', 3,
 ( #10711, #11974, #4592, #7372, #3546, #10868, #15647, #14274, #14524, #1001, #6186, #9521, #7139, #1082, #2185, #4749, #3624, #14610 ),
 .UNSPECIFIED., .F., .F.,
 ( 4, 2, 2, 2, 2, 2, 2, 2, 4 ),
 ( 0.003131918686235958278, 0.003523310662250251149, 0.003914702638264544454, 0.004306094614278836892, 0.004697486590293130197, 0.005088878566307422635, 0.005480270542321715940, 0.005871662518336009245, 0.006263054494350301683 ),
 .UNSPECIFIED. ) ;
#3047 = CARTESIAN_POINT ( 'NONE',  ( 2.094888798833199608E-14, -6.000000000000000888, 30.00000000000000000 ) ) ;
#3048 = CARTESIAN_POINT ( 'NONE',  ( -4.291255145204075916, 4.544933371694674484, 31.61396179408071561 ) ) ;
#3049 = CARTESIAN_POINT ( 'NONE',  ( 1.035533905932738197, 187.7499999978150527, 9.500000000000000000 ) ) ;
#3050 = CARTESIAN_POINT ( 'NONE',  ( 1.767766952966369098, 187.9999999978150527, 5.232233047033630235 ) ) ;
#3051 = CARTESIAN_POINT ( 'NONE',  ( 2.500000000000000444, 184.6999999978150697, 7.000000000000000000 ) ) ;
#3052 = CARTESIAN_POINT ( 'NONE',  ( 5.621197618055726153, 2.101623592078383673, 18.97398020122238904 ) ) ;
#3053 = ITEM_DEFINED_TRANSFORMATION ( 'NONE', 'NONE', #14221,  #14201 ) ;
#3054 = CARTESIAN_POINT ( 'NONE',  ( 2.500000000000000444, 188.8199999975965682, 5.964466094067262247 ) ) ;
#3055 = CARTESIAN_POINT ( 'NONE',  ( -1.691178964804313178, 228.6047289695326583, 7.985882612257780622 ) ) ;
#3056 = CARTESIAN_POINT ( 'NONE',  ( 2.817313151350985034, 5.579000502529534167, 17.99999999999998934 ) ) ;
#3057 = ORIENTED_EDGE ( 'NONE', *, *, #6193, .T. ) ;
#3058 = CARTESIAN_POINT ( 'NONE',  ( -1.224708070464005871, -2.198689805042928658, -2.500577006192093332 ) ) ;
#3059 = SHAPE_REPRESENTATION ( 'silicon body', ( #14201 ), #2994 ) ;
#3060 = ORIENTED_EDGE ( 'NONE', *, *, #8685, .T. ) ;
#3061 = CARTESIAN_POINT ( 'NONE',  ( 3.458623254138784908, -5.207221900902769818, 5.973772828752683672 ) ) ;
#3062 = LINE ( 'NONE', #12755, #5347 ) ;
#3063 = CARTESIAN_POINT ( 'NONE',  ( 2.066987300000000527, 184.2499999989074979, 7.000000000000000000 ) ) ;
#3064 = CARTESIAN_POINT ( 'NONE',  ( 5.903596343266329427, 2.055998103990495540, 23.50004921015706216 ) ) ;
#3065 = CARTESIAN_POINT ( 'NONE',  ( -5.866984344570831844, 1.259800266528639190, 17.20068193741824558 ) ) ;
#3066 = CARTESIAN_POINT ( 'NONE',  ( 5.317509234264027107, 2.779225709350867213, 24.49999999999999289 ) ) ;
#3067 = CARTESIAN_POINT ( 'NONE',  ( 0.000000000000000000, 184.0000000000000000, 0.000000000000000000 ) ) ;
#3068 = CARTESIAN_POINT ( 'NONE',  ( -2.500000000000000444, 1.035533905932737753, 0.05000000000000014155 ) ) ;
#3069 = CARTESIAN_POINT ( 'NONE',  ( 0.000000000000000000, 184.0000000000000000, 7.000000000000000000 ) ) ;
#3070 = CARTESIAN_POINT ( 'NONE',  ( 1.035533905932737531, 2.500000000000000444, 1.550000002184949821 ) ) ;
#3071 = CARTESIAN_POINT ( 'NONE',  ( 1.767766952966368432, 187.8999999999999773, 8.767766952966368876 ) ) ;
#3072 = EDGE_CURVE ( 'NONE', #1584, #2830, #8526, .T. ) ;
#3073 = CARTESIAN_POINT ( 'NONE',  ( 1.052850409966403333, 227.7074407335792614, 5.394463008855642450 ) ) ;
#3074 = PRODUCT_DEFINITION_CONTEXT ( 'detailed design', #12070, 'design' ) ;
#3075 = CARTESIAN_POINT ( 'NONE',  ( 0.000000000000000000, 19.99999999999999645, 0.000000000000000000 ) ) ;
#3076 = B_SPLINE_CURVE_WITH_KNOTS ( 'NONE', 3,
 ( #3288, #8152, #6961, #4569, #9419, #14254, #8230, #7037, #11867, #3970, #13911, #5180, #11448, #3022, #472, #1818, #10186, #4133 ),
 .UNSPECIFIED., .F., .F.,
 ( 4, 2, 2, 2, 2, 2, 2, 2, 4 ),
 ( 0.003131918686235976492, 0.003523310662250265894, 0.003914702638264555730, 0.004306094614278844698, 0.004697486590293134534, 0.005088878566307424370, 0.005480270542321714206, 0.005871662518336004041, 0.006263054494350294744 ),
 .UNSPECIFIED. ) ;
#3077 = CARTESIAN_POINT ( 'NONE',  ( 6.143020266950986574, -1.155160780047669755, 30.38558052754516225 ) ) ;
#3078 = CARTESIAN_POINT ( 'NONE',  ( 2.066987300000000083, -0.8561741729129450640, -0.7999999989075252671 ) ) ;
#3079 = CARTESIAN_POINT ( 'NONE',  ( 2.500000000000000000, 188.7500000000000000, 8.035533905932739529 ) ) ;
#3080 = CYLINDRICAL_SURFACE ( 'NONE', #12155, 1.000000000000000666 ) ;
#3082 = ORIENTED_EDGE ( 'NONE', *, *, #1490, .T. ) ;
#3081 = DIRECTION ( 'NONE',  ( -1.000000000000000000, 3.326610055774637112E-18, 1.062480551894331163E-17 ) ) ;
#3083 = CARTESIAN_POINT ( 'NONE',  ( 2.126728311762493157E-16, 22.00000000000000000, 8.250000000000003553 ) ) ;
#3084 = CARTESIAN_POINT ( 'NONE',  ( -9.750000000000003553, 22.00000000000000000, -3.401296724241641415E-14 ) ) ;
#3085 = B_SPLINE_CURVE_WITH_KNOTS ( 'NONE', 3,
 ( #6561, #14906, #7739, #5289, #14755, #9901, #1375, #11165, #12510, #1533, #11397, #5049, #7509, #14989, #265, #2889, #10058, #11321 ),
 .UNSPECIFIED., .F., .F.,
 ( 4, 2, 2, 2, 2, 2, 2, 2, 4 ),
 ( 0.003131486019301992028, 0.003522824630466698734, 0.003914163241631405006, 0.004305501852796111278, 0.004696840463960818418, 0.005088179075125524690, 0.005479517686290230963, 0.005870856297454938102, 0.006262194908619644375 ),
 .UNSPECIFIED. ) ;
#3086 = PLANE ( 'NONE',  #12655 ) ;
#3087 = ADVANCED_FACE ( 'NONE', ( #13355 ), #5220, .T. ) ;
#3088 = CARTESIAN_POINT ( 'NONE',  ( 2.757857370799680297, 189.3567818799732549, 5.841158458801078979 ) ) ;
#3089 = CARTESIAN_POINT ( 'NONE',  ( -9.825582188149883933E-17, 188.0999999978150754, 4.500000000000000000 ) ) ;
#3090 = CARTESIAN_POINT ( 'NONE',  ( -0.2612047379802446279, 227.6089814726536531, 5.110107047554619975 ) ) ;
#3091 = CARTESIAN_POINT ( 'NONE',  ( 1.965304387191771029, 228.1545866171788930, 6.685845824222668377 ) ) ;
#3092 = CARTESIAN_POINT ( 'NONE',  ( 5.571002711501508387, -2.833546409886088302, 24.23620383159193636 ) ) ;
#3093 = CARTESIAN_POINT ( 'NONE',  ( -6.176542424588120639, 0.9554180641285460185, 5.000000000000004441 ) ) ;
#3094 = VECTOR ( 'NONE', #14694, 1000.000000000000000 ) ;
#3095 = CARTESIAN_POINT ( 'NONE',  ( 2.999999999999999556, 1.732050807568877859, -5.500000000000000000 ) ) ;
#3096 = ORIENTED_EDGE ( 'NONE', *, *, #4101, .F. ) ;
#3097 = CARTESIAN_POINT ( 'NONE',  ( -0.8561741729129469514, 184.7999999989075093, 9.066987300000000971 ) ) ;
#3098 = PRODUCT_DEFINITION_SHAPE ( 'NONE', 'NONE',  #15743 ) ;
#3099 = CARTESIAN_POINT ( 'NONE',  ( -0.2619456584321428472, 5.995505046955617701, 10.52607193928646545 ) ) ;
#3100 = ORIENTED_EDGE ( 'NONE', *, *, #7862, .T. ) ;
#3101 = DIRECTION ( 'NONE',  ( 0.000000000000000000, 0.000000000000000000, -1.000000000000000000 ) ) ;
#3102 =( NAMED_UNIT ( * ) SI_UNIT ( $, .STERADIAN. ) SOLID_ANGLE_UNIT ( ) );
#3103 = AXIS2_PLACEMENT_3D ( 'NONE', #6546, #170, #2797 ) ;
#3104 = CARTESIAN_POINT ( 'NONE',  ( -4.286401442266531525, -4.198423832313195270, 5.000000000000004441 ) ) ;
#3105 = CARTESIAN_POINT ( 'NONE',  ( 0.2623718222035977821, 6.245654667075780431, 10.52627829713834018 ) ) ;
#3106 =( NAMED_UNIT ( * ) SI_UNIT ( $, .STERADIAN. ) SOLID_ANGLE_UNIT ( ) );
#3107 = CARTESIAN_POINT ( 'NONE',  ( 5.375913338529189289, -2.664979843780238777, 23.99571079637979665 ) ) ;
#3108 = CARTESIAN_POINT ( 'NONE',  ( -1.035533905932738197, -2.500000000000000000, -1.350000000000000089 ) ) ;
#3109 = CARTESIAN_POINT ( 'NONE',  ( 1.354942164306246880E-13, -6.000000000000000888, 16.99999999999998579 ) ) ;
#3110 = CARTESIAN_POINT ( 'NONE',  ( 0.000000000000000000, 222.7460571280668091, 12.08513476933103625 ) ) ;
#3111 = DIRECTION ( 'NONE',  ( 0.000000000000000000, -1.000000000000000000, 0.000000000000000000 ) ) ;
#3112 = CARTESIAN_POINT ( 'NONE',  ( 3.254737477227979792, 5.337033878705218726, 31.87367328635992791 ) ) ;
#3113 = EDGE_CURVE ( 'NONE', #5590, #13467, #11017, .T. ) ;
#3114 = CARTESIAN_POINT ( 'NONE',  ( -2.710505431213761085E-17, 228.2551366889530016, 10.16828399152529983 ) ) ;
#3115 = EDGE_CURVE ( 'NONE', #9879, #2165, #193, .T. ) ;
#3116 = ORIENTED_EDGE ( 'NONE', *, *, #5417, .T. ) ;
#3117 = ORIENTED_EDGE ( 'NONE', *, *, #5811, .F. ) ;
#3118 = EDGE_CURVE ( 'NONE', #4626, #1119, #947, .T. ) ;
#3119 = ORIENTED_EDGE ( 'NONE', *, *, #7586, .T. ) ;
#3120 = CARTESIAN_POINT ( 'NONE',  ( 4.290130679986573270, -4.545972905167727340, 12.11560192892920718 ) ) ;
#3121 = DIRECTION ( 'NONE',  ( 0.000000000000000000, 1.000000000000000000, 0.000000000000000000 ) ) ;
#3122 = ORIENTED_EDGE ( 'NONE', *, *, #2307, .T. ) ;
#3123 = CARTESIAN_POINT ( 'NONE',  ( 1.035533905932737531, 2.500000000000000444, 0.7500000021849494436 ) ) ;
#3124 = CARTESIAN_POINT ( 'NONE',  ( -2.500000000000000000, 0.000000000000000000, -2.199999997815050623 ) ) ;
#3125 = FACE_OUTER_BOUND ( 'NONE', #13175, .T. ) ;
#3126 = CARTESIAN_POINT ( 'NONE',  ( -7.826584432629735133E-16, 189.2999999978150356, 9.500000000000001776 ) ) ;
#3127 = AXIS2_PLACEMENT_3D ( 'NONE', #13077, #14347, #15560 ) ;
#3128 = CARTESIAN_POINT ( 'NONE',  ( 1.035533905932739085, -2.500000000000000000, 1.956999999978150662 ) ) ;
#3129 = DIRECTION ( 'NONE',  ( 0.9510565162951500895, 0.3090169943749582204, 0.000000000000000000 ) ) ;
#3130 = APPLICATION_PROTOCOL_DEFINITION ( 'draft international standard', 'automotive_design', 1998, #13184 ) ;
#3131 = CARTESIAN_POINT ( 'NONE',  ( 1.461580736456472573, 1.461580736456472795, 1.750000001092474999 ) ) ;
#3132 = CARTESIAN_POINT ( 'NONE',  ( -1.767766952966369765, 188.4699999975965738, 8.767766952966368876 ) ) ;
#3133 = CARTESIAN_POINT ( 'NONE',  ( 2.189302528786933877, 227.9503441805575505, 9.272039875547573473 ) ) ;
#3134 = CARTESIAN_POINT ( 'NONE',  ( -1.586193948774629714, 228.1096603596491832, 9.740555404025270647 ) ) ;
#3135 = EDGE_CURVE ( 'NONE', #8762, #10770, #8481, .T. ) ;
#3136 = VERTEX_POINT ( 'NONE', #8994 ) ;
#3137 = CARTESIAN_POINT ( 'NONE',  ( 2.135184931484484849, 1.332301797266478571, -2.499207808506416661 ) ) ;
#3138 = AXIS2_PLACEMENT_3D ( 'NONE', #12731, #11387, #10129 ) ;
#3139 = ORIENTED_EDGE ( 'NONE', *, *, #9122, .T. ) ;
#3140 = DIRECTION ( 'NONE',  ( 0.8090169943749421222, 0.5877852522924802425, 0.000000000000000000 ) ) ;
#3141 = CARTESIAN_POINT ( 'NONE',  ( -2.500000000000001776, 189.1499999978151152, 8.035533905932737753 ) ) ;
#3142 = DIRECTION ( 'NONE',  ( 1.000000000000000000, 0.000000000000000000, 0.000000000000000000 ) ) ;
#3143 = VERTEX_POINT ( 'NONE', #14281 ) ;
#3144 = DIRECTION ( 'NONE',  ( 0.000000000000000000, 1.000000000000000000, 0.000000000000000000 ) ) ;
#3145 = FACE_OUTER_BOUND ( 'NONE', #14163, .T. ) ;
#3146 = CARTESIAN_POINT ( 'NONE',  ( 2.500000000000000444, -1.035533905932737309, -0.3500000000000000333 ) ) ;
#3147 = CARTESIAN_POINT ( 'NONE',  ( 4.195795028115047565, 4.289273350251304073, 4.495710796379801089 ) ) ;
#3148 =( NAMED_UNIT ( * ) SI_UNIT ( $, .STERADIAN. ) SOLID_ANGLE_UNIT ( ) );
#3149 = VECTOR ( 'NONE', #2942, 1000.000000000000000 ) ;
#3150 = CARTESIAN_POINT ( 'NONE',  ( 0.05609725182637026464, 0.4000000000000045186, -2.541957560783562720 ) ) ;
#3151 = CARTESIAN_POINT ( 'NONE',  ( 1.767766952966368432, 188.7000000000000171, 8.767766952966368876 ) ) ;
#3152 = CARTESIAN_POINT ( 'NONE',  ( 1.826454486347603767, 228.0556294925947896, 9.581672574142119814 ) ) ;
#3153 = FACE_BOUND ( 'NONE', #12056, .T. ) ;
#3154 = CARTESIAN_POINT ( 'NONE',  ( 0.000000000000000000, 6.250000000000000888, 25.49999999999999645 ) ) ;
#3155 = CARTESIAN_POINT ( 'NONE',  ( -1.461580736456472351, -1.461580736456473018, -2.649999998907525356 ) ) ;
#3156 = CARTESIAN_POINT ( 'NONE',  ( -1.767766952966369765, 186.9000000000000057, 8.767766952966368876 ) ) ;
#3157 = CARTESIAN_POINT ( 'NONE',  ( 4.435347140100928343, -4.403429997944614982, 24.49999999999999289 ) ) ;
#3159 = ORIENTED_EDGE ( 'NONE', *, *, #10911, .T. ) ;
#3158 = CARTESIAN_POINT ( 'NONE',  ( 5.935543223013846514, 0.8771126767607477781, 5.000000000000004441 ) ) ;
#3160 = DIRECTION ( 'NONE',  ( 1.000000000000000000, 0.000000000000000000, 0.000000000000000000 ) ) ;
#3161 = CARTESIAN_POINT ( 'NONE',  ( -5.783239563508382197, 1.602707436861265267, 23.52641404563304661 ) ) ;
#3162 = CARTESIAN_POINT ( 'NONE',  ( -0.1882270327582609148, 228.2551366869376182, 10.16828399218531587 ) ) ;
#3163 = CARTESIAN_POINT ( 'NONE',  ( 6.176542424588135738, 0.9554180641284293340, 24.63060690723497359 ) ) ;
#3164 = CARTESIAN_POINT ( 'NONE',  ( -2.500000000000000444, 184.3300000002185186, 7.000000000000000000 ) ) ;
#3165 = CARTESIAN_POINT ( 'NONE',  ( -1.214607412227127980, 227.7425047733634642, 5.495729955674467426 ) ) ;
#3166 = CARTESIAN_POINT ( 'NONE',  ( 0.3231974900581740529, 228.9035839249116009, 8.848992768962338218 ) ) ;
#3167 = DIRECTION ( 'NONE',  ( 0.000000000000000000, 0.000000000000000000, -1.000000000000000000 ) ) ;
#3168 = CARTESIAN_POINT ( 'NONE',  ( -6.142908455506956855, 1.155755562475985654, 4.384822196241565884 ) ) ;
#3169 = B_SPLINE_CURVE_WITH_KNOTS ( 'NONE', 3,
 ( #5541, #8080, #12839, #1942, #753, #3297 ),
 .UNSPECIFIED., .F., .F.,
 ( 4, 2, 4 ),
 ( 0.1250000000000000000, 0.1875000000000000000, 0.2500000000000000000 ),
 .UNSPECIFIED. ) ;
#3170 = CARTESIAN_POINT ( 'NONE',  ( -3.735642931250987342, -4.696778275484508214, 30.02591947216899371 ) ) ;
#3171 = VERTEX_POINT ( 'NONE', #15257 ) ;
#3172 = CARTESIAN_POINT ( 'NONE',  ( -2.066987300000001415, 185.4999999989075548, 7.856174172912944620 ) ) ;
#3173 = DIRECTION ( 'NONE',  ( 1.062480551894329776E-17, 2.775557561562888393E-16, -1.000000000000000000 ) ) ;
#3174 = ADVANCED_FACE ( 'NONE', ( #4359 ), #3086, .F. ) ;
#3175 = EDGE_LOOP ( 'NONE', ( #5886, #5946, #4607, #11234, #14651, #4654, #3423, #5027 ) ) ;
#3176 = ADVANCED_FACE ( 'NONE', ( #850 ), #7066, .T. ) ;
#3177 = DIRECTION ( 'NONE',  ( -0.000000000000000000, 1.000000000000000000, -0.000000000000000000 ) ) ;
#3178 = CARTESIAN_POINT ( 'NONE',  ( -2.692693252389511294, -5.362085866495146291, 5.263826032055955118 ) ) ;
#3179 = CARTESIAN_POINT ( 'NONE',  ( -2.066987300000000971, 184.8999999989075320, 7.856174172912944620 ) ) ;
#3180 = EDGE_CURVE ( 'NONE', #10913, #9483, #1348, .T. ) ;
#3181 = DIRECTION ( 'NONE',  ( -6.123233995736766036E-17, 1.000000000000000000, 0.000000000000000000 ) ) ;
#3182 = FILL_AREA_STYLE_COLOUR ( '', #3534 ) ;
#3183 = CARTESIAN_POINT ( 'NONE',  ( 5.330189595673735958, -2.755293208590051890, 24.23617396794404044 ) ) ;
#3184 = CARTESIAN_POINT ( 'NONE',  ( 1.035533905932739085, -2.500000000000000000, -0.3499999978150501456 ) ) ;
#3185 = FACE_OUTER_BOUND ( 'NONE', #8944, .T. ) ;
#3186 = CARTESIAN_POINT ( 'NONE',  ( 5.999999999999999112, 189.3270225533669020, 3.938484906660877805 ) ) ;
#3187 = AXIS2_PLACEMENT_3D ( 'NONE', #6012, #3374, #8241 ) ;
#3188 = LINE ( 'NONE', #10353, #3417 ) ;
#3189 = CARTESIAN_POINT ( 'NONE',  ( -5.330004929009514392, -2.755647751839538806, 17.73760108194401752 ) ) ;
#3190 = CARTESIAN_POINT ( 'NONE',  ( -0.05145228733558462192, 189.6978048838913651, 10.38925534086671654 ) ) ;
#3191 = ORIENTED_EDGE ( 'NONE', *, *, #14382, .F. ) ;
#3192 = ORIENTED_EDGE ( 'NONE', *, *, #4450, .T. ) ;
#3193 = ORIENTED_EDGE ( 'NONE', *, *, #10472, .F. ) ;
#3194 = CARTESIAN_POINT ( 'NONE',  ( 2.817313151351127143, -5.579000502529464889, 11.63060690723496116 ) ) ;
#3195 = DIRECTION ( 'NONE',  ( 0.000000000000000000, 0.000000000000000000, -1.000000000000000000 ) ) ;
#3196 = B_SPLINE_CURVE_WITH_KNOTS ( 'NONE', 3,
 ( #2197, #3163, #3392, #9532, #2119, #9373, #4440, #12858, #2043, #14211, #13020, #5794, #15502, #4600, #11903, #8260, #1012, #7068 ),
 .UNSPECIFIED., .F., .F.,
 ( 4, 2, 2, 2, 2, 2, 2, 2, 4 ),
 ( 0.003131486019301973813, 0.003522824630466683121, 0.003914163241631392863, 0.004305501852796101737, 0.004696840463960811479, 0.005088179075125520354, 0.005479517686290230095, 0.005870856297454939837, 0.006262194908619648712 ),
 .UNSPECIFIED. ) ;
#3197 = ORIENTED_EDGE ( 'NONE', *, *, #7064, .T. ) ;
#3198 = DIRECTION ( 'NONE',  ( -0.000000000000000000, 1.000000000000000000, -0.000000000000000000 ) ) ;
#3199 = CARTESIAN_POINT ( 'NONE',  ( -2.500000000000000444, 1.035533905932737753, -0.6499999978150502455 ) ) ;
#3200 = CARTESIAN_POINT ( 'NONE',  ( 5.985119669071130133, 1.805077827356515341, 18.99991741810287493 ) ) ;
#3201 = FACE_OUTER_BOUND ( 'NONE', #9464, .T. ) ;
#3202 = CARTESIAN_POINT ( 'NONE',  ( -2.066987300000000083, 185.6499999989075320, 7.000000000000000000 ) ) ;
#3203 = CARTESIAN_POINT ( 'NONE',  ( 1.767766952966368654, 1.767766952966369098, 1.406999999978150617 ) ) ;
#3204 = CARTESIAN_POINT ( 'NONE',  ( 5.375913338529122676, 2.664979843780374669, 18.50428920362019625 ) ) ;
#3205 = CARTESIAN_POINT ( 'NONE',  ( -2.066987299999999195, -0.8561741729129466183, 0.5000000010924746663 ) ) ;
#3206 = CARTESIAN_POINT ( 'NONE',  ( 1.767766952966369098, 189.6699999975965341, 5.232233047033630235 ) ) ;
#3207 = CARTESIAN_POINT ( 'NONE',  ( 2.600554376340839635, 226.8075635770346139, 5.908288162427849599 ) ) ;
#3208 = VERTEX_POINT ( 'NONE', #10486 ) ;
#3209 = CARTESIAN_POINT ( 'NONE',  ( 3.736691294293501109, -4.695920479336315623, 4.026414045633067040 ) ) ;
#3210 = ORIENTED_EDGE ( 'NONE', *, *, #1750, .F. ) ;
#3211 = DIRECTION ( 'NONE',  ( 0.000000000000000000, -2.775557561562888393E-16, 1.000000000000000000 ) ) ;
#3212 = CARTESIAN_POINT ( 'NONE',  ( -5.935543223013861613, 0.8771126767606655106, 5.000000000000004441 ) ) ;
#3213 = CARTESIAN_POINT ( 'NONE',  ( -0.9740807849836103927, 5.920620690450690837, 4.738501197006693921 ) ) ;
#3214 = EDGE_CURVE ( 'NONE', #15454, #9028, #4514, .T. ) ;
#3215 = VERTEX_POINT ( 'NONE', #8101 ) ;
#3216 = LINE ( 'NONE', #13072, #14785 ) ;
#3217 = AXIS2_PLACEMENT_3D ( 'NONE', #15248, #15406, #11580 ) ;
#3218 = CARTESIAN_POINT ( 'NONE',  ( 2.283493650000000041, 184.5749999983613066, 7.000000000000000000 ) ) ;
#3219 = CARTESIAN_POINT ( 'NONE',  ( 1.035533905932737531, 2.500000000000000444, -0.9500000000000001776 ) ) ;
#3220 = DIRECTION ( 'NONE',  ( 1.000000000000000000, -1.251928832280965695E-16, 0.000000000000000000 ) ) ;
#3221 = SHAPE_REPRESENTATION_RELATIONSHIP ( 'NONE' , 'NONE' ,  #5305, #10501 ) ;
#3222 = CARTESIAN_POINT ( 'NONE',  ( 5.317509234263932072, 2.779225709351047957, 5.000000000000004441 ) ) ;
#3223 = CARTESIAN_POINT ( 'NONE',  ( 2.500000000000000444, 185.4999999978150527, 7.000000000000000000 ) ) ;
#3224 = B_SPLINE_CURVE_WITH_KNOTS ( 'NONE', 3,
 ( #8127, #4706, #3190, #3501, #15605, #4623 ),
 .UNSPECIFIED., .F., .F.,
 ( 4, 2, 4 ),
 ( 0.01906023950618289733, 0.01909837383777384864, 0.01913650816936479995 ),
 .UNSPECIFIED. ) ;
#3225 = CARTESIAN_POINT ( 'NONE',  ( -1.498122667687309173, 228.6899413643594983, 8.231980868713440813 ) ) ;
#3226 = CARTESIAN_POINT ( 'NONE',  ( 6.176542424588140179, -0.9554180641284089059, 17.99999999999998934 ) ) ;
#3227 = CARTESIAN_POINT ( 'NONE',  ( -5.665308849928801571, 1.980336949702567129, 18.99992002356260912 ) ) ;
#3228 = CARTESIAN_POINT ( 'NONE',  ( -1.461580736456472795, 1.461580736456472795, -0.4499999989075252338 ) ) ;
#3229 = CARTESIAN_POINT ( 'NONE',  ( -1.035533905932739751, 187.7500000000000284, 9.500000000000003553 ) ) ;
#3230 = CARTESIAN_POINT ( 'NONE',  ( -3.158825713737709595, 5.393784879207039751, 25.29933148907577944 ) ) ;
#3232 = ORIENTED_EDGE ( 'NONE', *, *, #13510, .T. ) ;
#3231 = CARTESIAN_POINT ( 'NONE',  ( -2.500000000000000444, 1.035533905932737753, -1.449999997815050401 ) ) ;
#3233 = CARTESIAN_POINT ( 'NONE',  ( -5.570820891630761551, 2.833901239560411955, 18.26236973443873168 ) ) ;
#3234 = PRODUCT_DEFINITION_FORMATION_WITH_SPECIFIED_SOURCE ( 'ANY', '', #6900, .NOT_KNOWN. ) ;
#3235 = VECTOR ( 'NONE', #187, 1000.000000000000227 ) ;
#3236 = CARTESIAN_POINT ( 'NONE',  ( -5.131373506000769247, 7.062729720843990755, 11.49999999999998224 ) ) ;
#3237 = CARTESIAN_POINT ( 'NONE',  ( -2.966128040510949582, 227.4385277522438287, 7.766262359440736951 ) ) ;
#3238 = CARTESIAN_POINT ( 'NONE',  ( 0.5294602902338498840, 189.4400223437018553, 4.020063421733246933 ) ) ;
#3239 = CARTESIAN_POINT ( 'NONE',  ( 1.767766952966369320, 184.0300000002184788, 5.232233047033630235 ) ) ;
#3240 = CARTESIAN_POINT ( 'NONE',  ( -5.915653884842702936, -1.003805156977440438, 5.504397606442129387 ) ) ;
#3241 = CARTESIAN_POINT ( 'NONE',  ( 1.984332343511774788, 228.2073501340537973, 6.838229870390527765 ) ) ;
#3242 = CYLINDRICAL_SURFACE ( 'NONE', #1896, 6.000000000000000888 ) ;
#3243 = DIRECTION ( 'NONE',  ( -0.000000000000000000, 1.000000000000000000, -0.000000000000000000 ) ) ;
#3244 = CARTESIAN_POINT ( 'NONE',  ( 0.5031281619707989039, 5.980084330432664963, 30.12602272744524967 ) ) ;
#3245 = EDGE_LOOP ( 'NONE', ( #7236, #2162, #2129, #10520 ) ) ;
#3246 = CARTESIAN_POINT ( 'NONE',  ( -2.066987300000000527, 184.6499999989075320, 7.000000000000000000 ) ) ;
#3247 = LINE ( 'NONE', #5648, #4274 ) ;
#3248 = AXIS2_PLACEMENT_3D ( 'NONE', #8997, #6375, #9148 ) ;
#3249 = ORIENTED_EDGE ( 'NONE', *, *, #6004, .F. ) ;
#3250 = CARTESIAN_POINT ( 'NONE',  ( -2.782713018890565770, -5.315928322779200244, 4.495602393557862619 ) ) ;
#3251 = CARTESIAN_POINT ( 'NONE',  ( 2.066987299999999639, 185.1999999989075150, 7.856174172912946396 ) ) ;
#3252 = CARTESIAN_POINT ( 'NONE',  ( 5.843075991566594851, 1.368655265451002911, 17.12635295315575590 ) ) ;
#3253 = CARTESIAN_POINT ( 'NONE',  ( -0.8561741729129469514, 185.5999999989074922, 9.066987300000000971 ) ) ;
#3254 = CIRCLE ( 'NONE', #13929, 2.649388036945190095 ) ;
#3255 = LINE ( 'NONE', #1749, #14025 ) ;
#3256 = CARTESIAN_POINT ( 'NONE',  ( 1.767766952966369320, -1.767766952966368654, -0.2999999978150504343 ) ) ;
#3257 = CARTESIAN_POINT ( 'NONE',  ( -5.984759433607005796, -1.806271833852304054, 3.999917806784440977 ) ) ;
#3258 = CARTESIAN_POINT ( 'NONE',  ( -5.999999999999999112, 221.4150671951173592, 6.196499129422101682 ) ) ;
#3259 = LINE ( 'NONE', #14305, #9529 ) ;
#3260 = CARTESIAN_POINT ( 'NONE',  ( 3.883716939929066303, 4.898343590941186321, 31.97359571723301741 ) ) ;
#3261 = CARTESIAN_POINT ( 'NONE',  ( -0.5042987395406310913, -5.979983180450088476, 18.87329304179975864 ) ) ;
#3262 = EDGE_CURVE ( 'NONE', #14829, #11779, #15713, .T. ) ;
#3263 = ORIENTED_EDGE ( 'NONE', *, *, #8275, .F. ) ;
#3264 = B_SPLINE_CURVE_WITH_KNOTS ( 'NONE', 3,
 ( #4108, #600, #14853, #8977, #2917, #11497, #6355, #1710, #5152, #290, #8815, #13644, #11806, #671, #994, #12763, #13079, #3222 ),
 .UNSPECIFIED., .F., .F.,
 ( 4, 2, 2, 2, 2, 2, 2, 2, 4 ),
 ( 0.003131918686235971722, 0.003523310662250261557, 0.003914702638264551393, 0.004306094614278841229, 0.004697486590293131065, 0.005088878566307420900, 0.005480270542321711603, 0.005871662518336001439, 0.006263054494350291275 ),
 .UNSPECIFIED. ) ;
#3265 = ORIENTED_EDGE ( 'NONE', *, *, #78, .T. ) ;
#3266 = AXIS2_PLACEMENT_3D ( 'NONE', #2520, #13173, #2592 ) ;
#3267 = ADVANCED_FACE ( 'NONE', ( #12778 ), #1882, .F. ) ;
#3268 = VERTEX_POINT ( 'NONE', #4437 ) ;
#3269 = CIRCLE ( 'NONE', #12168, 5.000000000000000000 ) ;
#3270 = CARTESIAN_POINT ( 'NONE',  ( 2.817313151351066747, -5.579000502529495975, 18.13060690723497004 ) ) ;
#3271 = DIRECTION ( 'NONE',  ( 0.000000000000000000, 1.000000000000000000, 0.000000000000000000 ) ) ;
#3272 = EDGE_LOOP ( 'NONE', ( #5512, #7097, #2471, #8178 ) ) ;
#3273 = CARTESIAN_POINT ( 'NONE',  ( 4.592425496802573972E-16, -2.500000000000000000, -0.3999999978150504676 ) ) ;
#3274 = ADVANCED_FACE ( 'NONE', ( #6914 ), #6989, .F. ) ;
#3275 = CARTESIAN_POINT ( 'NONE',  ( -5.317509234263918749, -2.779225709351067053, 31.13064961348856130 ) ) ;
#3276 = CARTESIAN_POINT ( 'NONE',  ( -4.152999119457922106, -4.671604476854401611, 4.199734849823242300 ) ) ;
#3277 = CARTESIAN_POINT ( 'NONE',  ( 2.500000000000000000, 189.4499999978150697, 8.035533905932739529 ) ) ;
#3278 = CARTESIAN_POINT ( 'NONE',  ( -1.767766952966368432, -1.767766952966369320, -0.5930000000218498268 ) ) ;
#3279 = CARTESIAN_POINT ( 'NONE',  ( 5.409423237179044719, 2.597448116730965317, 18.61561732698605454 ) ) ;
#3280 = ADVANCED_FACE ( 'NONE', ( #5716 ), #14315, .T. ) ;
#3281 = PRODUCT_CONTEXT ( 'NONE', #15331, 'mechanical' ) ;
#3282 = STYLED_ITEM ( 'NONE', ( #1539 ), #15531 ) ;
#3283 = CARTESIAN_POINT ( 'NONE',  ( -2.066987299999999639, 0.000000000000000000, -0.3499999989075254225 ) ) ;
#3284 = CARTESIAN_POINT ( 'NONE',  ( 4.416779112813715713, -4.422345839825735148, 4.737747182782874766 ) ) ;
#3285 = CARTESIAN_POINT ( 'NONE',  ( 2.843216347914732101, 226.9801049014886587, 6.416521247196312672 ) ) ;
#3286 = DIRECTION ( 'NONE',  ( -0.5877852522924685852, -0.8090169943749507819, 0.000000000000000000 ) ) ;
#3287 = VERTEX_POINT ( 'NONE', #1070 ) ;
#3288 = CARTESIAN_POINT ( 'NONE',  ( -5.317509234263873452, 2.779225709351156315, 24.49999999999999289 ) ) ;
#3289 = ORIENTED_EDGE ( 'NONE', *, *, #8249, .F. ) ;
#3290 = CARTESIAN_POINT ( 'NONE',  ( -1.000049271338417256, 6.169473353325564347, 11.36969612704547750 ) ) ;
#3291 = CARTESIAN_POINT ( 'NONE',  ( -1.084202172485504434E-16, 3.464101615137754830, -2.500000000000000000 ) ) ;
#3292 =( GEOMETRIC_REPRESENTATION_CONTEXT ( 3 ) GLOBAL_UNCERTAINTY_ASSIGNED_CONTEXT ( ( #9673 ) ) GLOBAL_UNIT_ASSIGNED_CONTEXT ( ( #2841, #8898, #7687 ) ) REPRESENTATION_CONTEXT ( 'NONE', 'WORKASPACE' ) );
#3293 = CARTESIAN_POINT ( 'NONE',  ( -0.8736516769106945635, 5.936271176698233454, 4.496067715786786323 ) ) ;
#3294 = ORIENTED_EDGE ( 'NONE', *, *, #1670, .T. ) ;
#3295 = CARTESIAN_POINT ( 'NONE',  ( 3.158296126777773605, 5.394094919772124186, 10.70112161576660270 ) ) ;
#3296 = CIRCLE ( 'NONE', #5081, 4.000000000000002665 ) ;
#3297 = CARTESIAN_POINT ( 'NONE',  ( -3.827021247335478803E-16, 2.500000000000000000, -2.500000000000000000 ) ) ;
#3298 = CARTESIAN_POINT ( 'NONE',  ( -2.817313151351250156, 5.579000502529401828, 11.63237410716304865 ) ) ;
#3299 = CARTESIAN_POINT ( 'NONE',  ( -2.500000000000000000, -1.035533905932739307, 0.1499999999999999667 ) ) ;
#3300 = DIRECTION ( 'NONE',  ( 0.8660254037844385966, -0.4999999999999998890, 0.000000000000000000 ) ) ;
#3301 = DIRECTION ( 'NONE',  ( -0.9510565162951544194, 0.3090169943749447312, 0.000000000000000000 ) ) ;
#3302 = CARTESIAN_POINT ( 'NONE',  ( -5.861467994999758346E-16, 186.0999999978150754, 9.500000000000001776 ) ) ;
#3304 = CARTESIAN_POINT ( 'NONE',  ( -2.913793338554793166E-15, 228.9118723800512782, 8.872930300147347182 ) ) ;
#3303 = AXIS2_PLACEMENT_3D ( 'NONE', #3693, #13399, #11016 ) ;
#3305 = CARTESIAN_POINT ( 'NONE',  ( -5.558508435838126260, -2.857531096719055252, 17.99999999999998934 ) ) ;
#3306 = EDGE_CURVE ( 'NONE', #10357, #11937, #5804, .T. ) ;
#3307 = VECTOR ( 'NONE', #9068, 1000.000000000000000 ) ;
#3308 = CARTESIAN_POINT ( 'NONE',  ( 2.817313151351047207, 5.579000502529503080, 11.49999999999998224 ) ) ;
#3309 = CARTESIAN_POINT ( 'NONE',  ( 0.8561741729129452860, 2.066987299999999639, -1.399999998907526022 ) ) ;
#3310 = PRODUCT_DEFINITION ( 'UNKNOWN', '', #4265, #6590 ) ;
#3311 = CARTESIAN_POINT ( 'NONE',  ( -2.500000000000000444, 186.8499999999999943, 8.035533905932737753 ) ) ;
#3312 = CARTESIAN_POINT ( 'NONE',  ( -3.255128505894475666, 5.336774832660618806, 25.37380055247395916 ) ) ;
#3313 = EDGE_CURVE ( 'NONE', #12601, #8963, #511, .T. ) ;
#3315 = ORIENTED_EDGE ( 'NONE', *, *, #1976, .T. ) ;
#3314 = DIRECTION ( 'NONE',  ( -0.5877852522924685852, -0.8090169943749508930, 0.000000000000000000 ) ) ;
#3316 = FACE_OUTER_BOUND ( 'NONE', #14983, .T. ) ;
#3317 = ORIENTED_EDGE ( 'NONE', *, *, #15341, .F. ) ;
#3318 = CARTESIAN_POINT ( 'NONE',  ( -5.903119516422456137, 1.077859910107602515, 23.88480617551148555 ) ) ;
#3319 = CARTESIAN_POINT ( 'NONE',  ( -1.530808498934191571E-16, 2.500000000000000000, -3.199999997815050623 ) ) ;
#3320 = FACE_OUTER_BOUND ( 'NONE', #6675, .T. ) ;
#3321 = CARTESIAN_POINT ( 'NONE',  ( -4.435347140101024266, -4.403429997944519947, 31.00000000000000000 ) ) ;
#3322 = CARTESIAN_POINT ( 'NONE',  ( 1.895314869936763680, 228.4599366835234093, 7.567714231851713436 ) ) ;
#3323 = CARTESIAN_POINT ( 'NONE',  ( 5.558508435838221295, 2.857531096718871844, 11.49999999999998224 ) ) ;
#3324 = DIRECTION ( 'NONE',  ( 1.000000000000000000, 0.000000000000000000, 0.000000000000000000 ) ) ;
#3325 = CARTESIAN_POINT ( 'NONE',  ( -2.500000000000000000, -1.035533905932739307, 1.050000002184949821 ) ) ;
#3326 = ORIENTED_EDGE ( 'NONE', *, *, #12016, .F. ) ;
#3327 = CARTESIAN_POINT ( 'NONE',  ( 2.066987300000000527, 185.0499999989075093, 7.000000000000000000 ) ) ;
#3328 = CARTESIAN_POINT ( 'NONE',  ( 3.106366801611981643, 5.134708448381295476, 30.12696220972948780 ) ) ;
#3329 = VERTEX_POINT ( 'NONE', #7129 ) ;
#3330 = CARTESIAN_POINT ( 'NONE',  ( -3.420659742068303810, -4.931142898501790661, 4.000049463537775907 ) ) ;
#3331 = CARTESIAN_POINT ( 'NONE',  ( -4.438452643612533777E-16, 185.0499999989075093, 9.066987300000000971 ) ) ;
#3332 = CARTESIAN_POINT ( 'NONE',  ( 5.866817325727523347, 1.260653813891904784, 17.19977782616120621 ) ) ;
#3333 = CARTESIAN_POINT ( 'NONE',  ( 1.461580736456472573, 187.3499999989074922, 8.461580736456474128 ) ) ;
#3334 = CARTESIAN_POINT ( 'NONE',  ( 4.005998022989861518, 4.467726698309353317, 18.79931806258173665 ) ) ;
#3335 = CARTESIAN_POINT ( 'NONE',  ( 1.767766952966368654, 1.767766952966369098, -0.09999999781505011787 ) ) ;
#3336 = CARTESIAN_POINT ( 'NONE',  ( 2.897581130414634077E-17, 22.00000000000000000, 11.25000000000000355 ) ) ;
#3337 = CARTESIAN_POINT ( 'NONE',  ( -5.999999999999999112, 186.5669965222008670, 9.317226423031115701 ) ) ;
#3338 = CARTESIAN_POINT ( 'NONE',  ( 4.286401442266591921, -4.198423832313132209, 5.000000000000004441 ) ) ;
#3339 = CARTESIAN_POINT ( 'NONE',  ( 1.461580736456473018, -1.461580736456472573, -2.249999998907525445 ) ) ;
#3340 = CARTESIAN_POINT ( 'NONE',  ( -0.8738118504724315949, -5.936246475285051005, 18.50357242174242600 ) ) ;
#3341 = EDGE_LOOP ( 'NONE', ( #8251, #9877 ) ) ;
#3342 = ORIENTED_EDGE ( 'NONE', *, *, #7064, .F. ) ;
#3343 = ORIENTED_EDGE ( 'NONE', *, *, #15674, .T. ) ;
#3344 = VECTOR ( 'NONE', #4978, 1000.000000000000000 ) ;
#3345 = CARTESIAN_POINT ( 'NONE',  ( 3.458623254138704084, 5.207221900902825773, 30.02622717124732077 ) ) ;
#3346 = CARTESIAN_POINT ( 'NONE',  ( -4.286401442266642547, 4.198423832313083359, 11.63064961348853288 ) ) ;
#3347 = ORIENTED_EDGE ( 'NONE', *, *, #11780, .F. ) ;
#3348 = PRODUCT_DEFINITION_SHAPE ( 'NONE', 'NONE',  #15765 ) ;
#3349 = EDGE_CURVE ( 'NONE', #9247, #8051, #2225, .T. ) ;
#3350 = CARTESIAN_POINT ( 'NONE',  ( 1.035533905932737531, 2.500000000000000444, -2.449999997815050179 ) ) ;
#3351 = CARTESIAN_POINT ( 'NONE',  ( 0.9999502950802097168, -5.916088184763882651, 5.131081491900111757 ) ) ;
#3352 = CARTESIAN_POINT ( 'NONE',  ( -3.458467055437195459, -5.207305717053890781, 4.026404282766992360 ) ) ;
#3353 = CARTESIAN_POINT ( 'NONE',  ( 1.035533905932737753, 188.0499999978150640, 4.500000000000000888 ) ) ;
#3354 = CARTESIAN_POINT ( 'NONE',  ( -2.500000000000000000, -1.035533905932739307, -0.6430000000218495382 ) ) ;
#3355 = CARTESIAN_POINT ( 'NONE',  ( 6.172614129015236983, -0.9817721000788701691, 4.737630265561252330 ) ) ;
#3356 = CARTESIAN_POINT ( 'NONE',  ( -0.8561741729129455081, 2.066987299999999639, 1.100000001092475088 ) ) ;
#3357 = VECTOR ( 'NONE', #3410, 1000.000000000000114 ) ;
#3358 = CARTESIAN_POINT ( 'NONE',  ( -1.035533905932737975, 188.2199999975965738, 4.500000000000000888 ) ) ;
#3359 = CARTESIAN_POINT ( 'NONE',  ( 2.923766376317260551, 227.0711491207812855, 6.684645050985161596 ) ) ;
#3360 = CARTESIAN_POINT ( 'NONE',  ( 2.500000000000000444, 1.035533905932737975, 0.6500000021849499099 ) ) ;
#3361 = EDGE_LOOP ( 'NONE', ( #8618, #4170 ) ) ;
#3362 = DIRECTION ( 'NONE',  ( 0.000000000000000000, 0.000000000000000000, 1.000000000000000000 ) ) ;
#3363 = VERTEX_POINT ( 'NONE', #8492 ) ;
#3364 = VERTEX_POINT ( 'NONE', #4902 ) ;
#3365 = DIRECTION ( 'NONE',  ( 0.000000000000000000, 9.159339953157539881E-15, -1.000000000000000000 ) ) ;
#3366 = EDGE_CURVE ( 'NONE', #9045, #3737, #4533, .T. ) ;
#3367 = CARTESIAN_POINT ( 'NONE',  ( -3.779082820360757378, -4.979770177899202288, 23.49995093123465750 ) ) ;
#3368 = LINE ( 'NONE', #10774, #9634 ) ;
#3369 = EDGE_LOOP ( 'NONE', ( #14239, #7079, #9, #6960 ) ) ;
#3370 = EDGE_CURVE ( 'NONE', #11100, #2054, #199, .T. ) ;
#3371 = CARTESIAN_POINT ( 'NONE',  ( -5.408775798201138407, 2.598833957129706551, 17.38602261056917087 ) ) ;
#3372 = CARTESIAN_POINT ( 'NONE',  ( 4.142173849413612885, 4.341773579105533187, 25.11519382448850379 ) ) ;
#3373 = CARTESIAN_POINT ( 'NONE',  ( 2.031800923367348393E-13, -6.250000000000000888, 23.49999999999999289 ) ) ;
#3374 = DIRECTION ( 'NONE',  ( -0.000000000000000000, 1.000000000000000000, -0.000000000000000000 ) ) ;
#3375 = CARTESIAN_POINT ( 'NONE',  ( -6.142844459177198679, -1.156093792145410193, 23.88439807107078039 ) ) ;
#3376 = CARTESIAN_POINT ( 'NONE',  ( 2.449293598294708880E-16, 2.000000000000000000, -15.50000000000000000 ) ) ;
#3377 = CARTESIAN_POINT ( 'NONE',  ( 12.50000000000000533, 1.530808498934192113E-15, 2.000000000000001776 ) ) ;
#3378 = CARTESIAN_POINT ( 'NONE',  ( 2.500000000000000000, 188.7999999999999829, 7.000000000000000000 ) ) ;
#3379 = CARTESIAN_POINT ( 'NONE',  ( -1.724643626337419855, 228.5864753960848077, 7.933165251024266063 ) ) ;
#3380 = CARTESIAN_POINT ( 'NONE',  ( -5.648559266344464369, -2.676764518776065138, 18.61396179408071205 ) ) ;
#3381 = AXIS2_PLACEMENT_3D ( 'NONE', #6549, #12656, #5275 ) ;
#3382 = PLANE ( 'NONE',  #7329 ) ;
#3383 = CARTESIAN_POINT ( 'NONE',  ( 2.500000000000000000, 187.9500000000000455, 8.035533905932739529 ) ) ;
#3384 = CARTESIAN_POINT ( 'NONE',  ( 0.000000000000000000, 2.000000000000000000, 0.000000000000000000 ) ) ;
#3385 = VERTEX_POINT ( 'NONE', #5429 ) ;
#3386 = CYLINDRICAL_SURFACE ( 'NONE', #479, 1.000000000000000666 ) ;
#3387 = CARTESIAN_POINT ( 'NONE',  ( -6.176542424588101099, 0.9554180641286806885, 18.13234125634167526 ) ) ;
#3388 = ORIENTED_EDGE ( 'NONE', *, *, #6253, .F. ) ;
#3389 = CIRCLE ( 'NONE', #4933, 1.500000000000000222 ) ;
#3390 = DIRECTION ( 'NONE',  ( 0.000000000000000000, 0.000000000000000000, 1.000000000000000000 ) ) ;
#3391 = CARTESIAN_POINT ( 'NONE',  ( -2.829488734775190473, 226.9686955073827619, 6.382877614595673599 ) ) ;
#3392 = CARTESIAN_POINT ( 'NONE',  ( 6.172614129015254747, 0.9817721000787504870, 24.76236973443873524 ) ) ;
#3393 = CARTESIAN_POINT ( 'NONE',  ( -1.035533905932739751, 186.0800000002184902, 9.500000000000003553 ) ) ;
#3394 = CARTESIAN_POINT ( 'NONE',  ( 1.979652835806277785E-15, 0.000000000000000000, 11.50000000000000000 ) ) ;
#3395 = CARTESIAN_POINT ( 'NONE',  ( -0.2610185499608090876, 227.6142484773064325, 5.125318457402467942 ) ) ;
#3396 = EDGE_CURVE ( 'NONE', #10225, #1897, #13336, .T. ) ;
#3397 = CYLINDRICAL_SURFACE ( 'NONE', #5473, 2.500000000000000000 ) ;
#3398 = CARTESIAN_POINT ( 'NONE',  ( 3.796994071234844259E-16, -2.066987299999999639, -0.7499999989075251117 ) ) ;
#3399 = CARTESIAN_POINT ( 'NONE',  ( 5.940390500375535510, 6.474944468551633747, 31.00000000000000000 ) ) ;
#3400 = VERTEX_POINT ( 'NONE', #1829 ) ;
#3401 = CARTESIAN_POINT ( 'NONE',  ( 2.066987299999999639, 188.9999999989074979, 7.856174172912946396 ) ) ;
#3402 = EDGE_CURVE ( 'NONE', #5247, #5666, #6779, .T. ) ;
#3403 = CARTESIAN_POINT ( 'NONE',  ( 4.286401442266448036, -4.198423832313277870, 24.49999999999999289 ) ) ;
#3404 = ORIENTED_EDGE ( 'NONE', *, *, #8079, .T. ) ;
#3405 = DIRECTION ( 'NONE',  ( -0.9510565162951545304, 0.3090169943749447867, 0.000000000000000000 ) ) ;
#3406 = EDGE_CURVE ( 'NONE', #3525, #2649, #14424, .T. ) ;
#3407 = CARTESIAN_POINT ( 'NONE',  ( -1.767766952966369098, 1.767766952966369098, 0.1000000021849497545 ) ) ;
#3408 = CARTESIAN_POINT ( 'NONE',  ( 4.290130679986468465, 4.545972905167828593, 17.38439807107078749 ) ) ;
#3409 = CARTESIAN_POINT ( 'NONE',  ( -1.461580736456473240, 186.1499999989075320, 5.538419263543526760 ) ) ;
#3410 = DIRECTION ( 'NONE',  ( 0.9510565162951499785, 0.3090169943749582204, 0.000000000000000000 ) ) ;
#3411 = CARTESIAN_POINT ( 'NONE',  ( -1.767766952966369098, 1.767766952966369098, -0.6999999978150501789 ) ) ;
#3412 = CARTESIAN_POINT ( 'NONE',  ( 0.000000000000000000, 0.000000000000000000, 2.500000000000000000 ) ) ;
#3413 = CARTESIAN_POINT ( 'NONE',  ( 3.659182332138577465E-16, 221.4150671951173308, 6.196499129422101682 ) ) ;
#3414 = CARTESIAN_POINT ( 'NONE',  ( -1.456896669277396583E-16, 188.8999999978150584, 4.500000000000000000 ) ) ;
#3415 = CARTESIAN_POINT ( 'NONE',  ( -2.500000000000001332, 185.1499999978150584, 8.035533905932735976 ) ) ;
#3416 = DIRECTION ( 'NONE',  ( -0.5877852522924685852, -0.8090169943749508930, 0.000000000000000000 ) ) ;
#3417 = VECTOR ( 'NONE', #564, 1000.000000000000000 ) ;
#3418 = ORIENTED_EDGE ( 'NONE', *, *, #3214, .T. ) ;
#3419 = ORIENTED_EDGE ( 'NONE', *, *, #5808, .F. ) ;
#3420 = VERTEX_POINT ( 'NONE', #2956 ) ;
#3421 = CARTESIAN_POINT ( 'NONE',  ( 3.882809187878927926, 4.899079348630055009, 30.02599901976670438 ) ) ;
#3422 = DIRECTION ( 'NONE',  ( 0.000000000000000000, 0.000000000000000000, 1.000000000000000000 ) ) ;
#3423 = ORIENTED_EDGE ( 'NONE', *, *, #10805, .F. ) ;
#3424 = CARTESIAN_POINT ( 'NONE',  ( 4.592425496802573972E-16, -2.500000000000000000, -1.999999997815050445 ) ) ;
#3425 = CARTESIAN_POINT ( 'NONE',  ( 0.5044069930203403107, -5.979990686694992341, 5.873357432279041390 ) ) ;
#3426 = PRESENTATION_LAYER_ASSIGNMENT (  '', '', ( #7001 ) ) ;
#3427 = DIRECTION ( 'NONE',  ( 0.000000000000000000, 0.000000000000000000, 1.000000000000000000 ) ) ;
#3428 = CARTESIAN_POINT ( 'NONE',  ( -1.084202172485504434E-16, 187.8499999989074922, 4.933012699999999029 ) ) ;
#3430 = CARTESIAN_POINT ( 'NONE',  ( -2.500000000000000000, 0.000000000000000000, -1.493000000021849516 ) ) ;
#3429 = B_SPLINE_CURVE_WITH_KNOTS ( 'NONE', 3,
 ( #6690, #624, #14220, #9382, #2128, #15196, #3328, #14295, #6927, #785, #11759, #938, #862, #15354, #5729, #10420, #8115, #11526 ),
 .UNSPECIFIED., .F., .F.,
 ( 4, 2, 2, 2, 2, 2, 2, 2, 4 ),
 ( 0.003131918686235979528, 0.003523310662250269364, 0.003914702638264559199, 0.004306094614278849035, 0.004697486590293139738, 0.005088878566307429574, 0.005480270542321720277, 0.005871662518336010980, 0.006263054494350301683 ),
 .UNSPECIFIED. ) ;
#3431 = CARTESIAN_POINT ( 'NONE',  ( 5.859155363331391975, -2.178872204144952196, 4.025999019766705267 ) ) ;
#3432 = ITEM_DEFINED_TRANSFORMATION ( 'NONE', 'NONE', #11687,  #14201 ) ;
#3433 = CARTESIAN_POINT ( 'NONE',  ( 2.066987299999999639, 0.8561741729129456191, -0.6999999989075255113 ) ) ;
#3434 = CARTESIAN_POINT ( 'NONE',  ( -1.767766952966369098, 1.767766952966369098, -2.399999999999999911 ) ) ;
#3435 = CARTESIAN_POINT ( 'NONE',  ( 2.994032664863047533, 227.2266946368854690, 7.142638454998203379 ) ) ;
#3436 = CARTESIAN_POINT ( 'NONE',  ( 5.903472034603470142, 2.056448723545269974, 6.000082193215566129 ) ) ;
#3437 = VERTEX_POINT ( 'NONE', #715 ) ;
#3438 = ORIENTED_EDGE ( 'NONE', *, *, #158, .F. ) ;
#3439 = AXIS2_PLACEMENT_3D ( 'NONE', #14275, #8253, #6909 ) ;
#3440 = CARTESIAN_POINT ( 'NONE',  ( -5.558508435838219519, 2.857531096718872732, 31.00000000000000000 ) ) ;
#3441 = ORIENTED_EDGE ( 'NONE', *, *, #2600, .T. ) ;
#3442 = EDGE_LOOP ( 'NONE', ( #5747, #15057, #6342, #8924, #3756, #8560, #12034, #14309, #801, #10670, #13109, #3467, #10485, #15607, #941, #11951 ) ) ;
#3443 = DIRECTION ( 'NONE',  ( 0.000000000000000000, 1.000000000000000000, 0.000000000000000000 ) ) ;
#3444 = CARTESIAN_POINT ( 'NONE',  ( 2.692143549875356534, -5.362363179736500562, 17.73805675996853637 ) ) ;
#3445 = CARTESIAN_POINT ( 'NONE',  ( -2.782769401326306902, -5.315896561274780829, 25.00428920362020335 ) ) ;
#3446 = ORIENTED_EDGE ( 'NONE', *, *, #3072, .F. ) ;
#3447 = CARTESIAN_POINT ( 'NONE',  ( -6.105925084677685355, -1.337450587213164566, 31.79933148907577234 ) ) ;
#3448 = UNCERTAINTY_MEASURE_WITH_UNIT (LENGTH_MEASURE( 1.000000000000000082E-05 ), #15296, 'distance_accuracy_value', 'NONE');
#3449 = CARTESIAN_POINT ( 'NONE',  ( 1.530808498934191324E-15, 184.0000000000000000, 12.49999999999999822 ) ) ;
#3450 = LINE ( 'NONE', #1298, #3344 ) ;
#3451 = CARTESIAN_POINT ( 'NONE',  ( 2.500000000000000444, -1.035533905932737309, -1.049999997815050268 ) ) ;
#3452 =( BOUNDED_CURVE ( )  B_SPLINE_CURVE ( 2, ( #4210, #1813, #6685, #10803, #4925, #58, #7234, #9780, #9537, #15584, #933, #10645, #13344, #12151, #14626, #1096, #12073, #8349, #3638, #13188, #4686, #8513, #14374, #11991, #3479, #5880, #2285, #3715, #14461, #7073, #9702, #8592, #2447, #15507, #13104, #6126, #4605, #13426, #1250, #7311, #10961, #5959, #7154, #3562, #9622, #9456, #15663, #4764, #1171, #8430, #5799, #10885, #2204, #2530, #10726, #11909, #7385, #6040, #13267, #14291, #3398, #2366, #8267, #6808, #4847, #14540, #1017, #3945, #14858, #136, #7535, #3868, #8903, #372, #2602, #10011, #8819, #2683, #9854, #12542, #9931, #13738, #6359, #220, #2846, #1481, #5240, #1639, #5156, #14782, #13574, #12462, #12382, #7617, #14703, #5001, #10164, #6440, #13649, #1326, #8981 ),
 .UNSPECIFIED., .F., .F. ) 
 B_SPLINE_CURVE_WITH_KNOTS ( ( 3, 2, 2, 2, 2, 2, 2, 2, 2, 2, 2, 2, 2, 2, 2, 2, 2, 2, 2, 2, 2, 2, 2, 2, 2, 2, 2, 2, 2, 2, 2, 2, 2, 2, 2, 2, 2, 2, 2, 2, 2, 2, 2, 2, 2, 2, 2, 2, 2, 2, 3 ),
 ( 0.000000000000000000, 0.01785714285714285615, 0.03571428571428571230, 0.05357142857142856845, 0.07142857142857142461, 0.08928571428571428770, 0.1071428571428571369, 0.1250000000000000000, 0.1428571428571428492, 0.1607142857142857262, 0.1785714285714285754, 0.1964285714285714246, 0.2142857142857142738, 0.2321428571428571508, 0.2500000000000000000, 0.2678571428571428492, 0.2857142857142856984, 0.3035714285714285476, 0.3214285714285714524, 0.3392857142857143016, 0.3571428571428571508, 0.3750000000000000000, 0.3928571428571428492, 0.4107142857142856984, 0.4285714285714285476, 0.4464285714285714524, 0.4642857142857143016, 0.4821428571428571508, 0.5000000000000000000, 0.5178571428571429047, 0.5357142857142856984, 0.5535714285714286031, 0.5714285714285713969, 0.5892857142857143016, 0.6071428571428570953, 0.6250000000000000000, 0.6428571428571429047, 0.6607142857142856984, 0.6785714285714286031, 0.6964285714285715079, 0.7142857142857143016, 0.7321428571428570953, 0.7500000000000000000, 0.7678571428571429047, 0.7857142857142856984, 0.8035714285714286031, 0.8214285714285713969, 0.8392857142857143016, 0.8571428571428570953, 0.8750000000000000000, 0.8928571428571429047 ),
 .UNSPECIFIED. ) 
 CURVE ( )  GEOMETRIC_REPRESENTATION_ITEM ( )  RATIONAL_B_SPLINE_CURVE ( ( 1.000000000000000000, 0.9238795325112867385, 1.000000000000000000, 0.9238795325112867385, 1.000000000000000000, 0.9238795325112867385, 1.000000000000000000, 0.9238795325112867385, 1.000000000000000000, 0.9238795325112867385, 1.000000000000000000, 0.9238795325112867385, 1.000000000000000000, 0.9238795325112867385, 1.000000000000000000, 0.9238795325112867385, 1.000000000000000000, 0.9238795325112867385, 1.000000000000000000, 0.9238795325112867385, 1.000000000000000000, 0.9238795325112867385, 1.000000000000000000, 0.9238795325112867385, 1.000000000000000000, 0.9238795325112867385, 1.000000000000000000, 0.9238795325112867385, 1.000000000000000000, 0.9238795325112867385, 1.000000000000000000, 0.9238795325112867385, 1.000000000000000000, 0.9238795325112867385, 1.000000000000000000, 0.9238795325112867385, 1.000000000000000000, 0.9238795325112867385, 1.000000000000000000, 0.9238795325112867385, 1.000000000000000000, 0.9238795325112867385, 1.000000000000000000, 0.9238795325112867385, 1.000000000000000000, 0.9238795325112867385, 1.000000000000000000, 0.9238795325112867385, 1.000000000000000000, 0.9238795325112867385, 1.000000000000000000, 0.9238795325112867385, 1.000000000000000000, 0.9238795325112867385, 1.000000000000000000, 0.9238795325112867385, 1.000000000000000000, 0.9238795325112867385, 1.000000000000000000, 0.9238795325112867385, 1.000000000000000000, 0.9238795325112867385, 1.000000000000000000, 0.9238795325112867385, 1.000000000000000000, 0.9238795325112867385, 1.000000000000000000, 0.9238795325112867385, 1.000000000000000000, 0.9238795325112867385, 1.000000000000000000, 0.9238795325112867385, 1.000000000000000000, 0.9238795325112867385, 1.000000000000000000, 0.9238795325112867385, 1.000000000000000000, 0.9238795325112867385, 1.000000000000000000, 0.9238795325112867385, 1.000000000000000000, 0.9238795325112867385, 1.000000000000000000, 0.9238795325112867385, 1.000000000000000000, 0.9238795325112867385, 1.000000000000000000, 0.9238795325112867385, 1.000000000000000000, 0.9238795325112867385, 1.000000000000000000, 0.9238795325112867385, 1.000000000000000000, 0.9238795325112867385, 1.000000000000000000, 0.9238795325112867385, 1.000000000000000000, 0.9238795325112867385, 1.000000000000000000, 0.9238795325112867385, 1.000000000000000000 ) ) 
 REPRESENTATION_ITEM ( '' )  );
#3453 = AXIS2_PLACEMENT_3D ( 'NONE', #12247, #3579, #1115 ) ;
#3454 = CARTESIAN_POINT ( 'NONE',  ( -5.769755079862221692, -2.405651898699208147, 23.62694108445698049 ) ) ;
#3455 = DIRECTION ( 'NONE',  ( 0.000000000000000000, 0.000000000000000000, 1.000000000000000000 ) ) ;
#3456 = B_SPLINE_SURFACE_WITH_KNOTS ( 'NONE', 1, 3, ( 
 ( #10179, #1888, #14137, #14058, #3166, #10492, #6683, #12784, #14214, #15423, #9225, #8024, #15505, #13985, #4603, #931, #4521, #9454, #4443, #4285, #14289, #5723, #5641, #9376, #9150, #7871, #618, #5797, #6842, #6763, #12712, #5490, #1811, #694, #12862, #10643, #3322, #1966, #6919, #11517, #10565, #9297, #10334, #11824, #11595, #5568, #10414, #15264, #3241, #15188, #3091, #7944, #8107, #8186, #4365, #11680, #13023, #779, #11753, #12946, #15346, #2046, #2122, #856, #6995, #11989, #8347, #4762, #15660, #10724, #5878, #1544, #9618, #7152, #5058, #9990, #8802, #13101, #12444, #3925, #11174, #274, #13265, #1094, #13185, #3395, #9535, #14458, #12071, #5957, #3560, #3849, #8428, #14765, #15582, #11906, #6419, #13555, #6259, #8264, #8722, #10801, #5137, #2283, #9911, #2364, #7232, #11097, #2202, #1384, #14839, #13631, #195, #2664, #11252, #14372, #353, #5218, #2745, #10068, #7517, #4684, #7071, #1460, #12363, #7596, #3476, #1015, #6338, #7986, #13865, #13792, #5607, #12521, #12826, #9115, #1930, #4247, #14917, #13946, #7906, #5376, #3055, #2977, #6649, #7674, #11406, #4007, #6804, #1620, #8886, #9040, #10223, #15152, #15226, #13718, #1852, #12748, #7828, #2825, #6496, #11639, #4329, #6726 ),
 ( #11331, #741, #12678, #5453, #507, #428, #11559, #5299, #10147, #4091, #1695, #12595, #15000, #6571, #656, #9187, #2901, #5528, #8961, #7750, #15074, #4168, #14027, #3133, #1776, #11481, #584, #10300, #10376, #9416, #12982, #13141, #10605, #10531, #4410, #5839, #2242, #15386, #11716, #2160, #7033, #9495, #11864, #892, #7113, #819, #14177, #3435, #4482, #9336, #14251, #3359, #7193, #3285, #2009, #6883, #13062, #3207, #11949, #8066, #8303, #974, #1054, #14328, #10685, #8227, #15545, #9264, #6958, #13228, #12032, #4642, #8391, #5918, #8148, #2085, #5684, #11791, #15307, #1131, #14099, #10765, #5762, #15620, #15464, #3520, #14415, #9573, #4724, #2320, #4566, #10454, #12908, #15702, #13540, #3833, #1441, #14501, #2648, #13613, #6241, #11002, #4885, #8475, #8555, #23, #9744, #14581, #13465, #8630, #258, #7347, #5118, #13379, #12424, #100, #2567, #8705, #12189, #3677, #10922, #5996, #12107, #2489, #14666, #1288, #6162, #11078, #4967, #1368, #13305, #3597, #3908, #177, #7424, #10839, #5041, #9818, #7501, #3755, #12268, #9894, #14747, #12346, #4804, #6319, #11156, #9972, #14823, #8783, #2725, #1208, #7577, #9660, #2404, #7272, #6079, #13695, #14005, #15133, #15055, #9096, #2805, #3114 ) ),
 .UNSPECIFIED., .F., .T., .F.,
 ( 2, 2 ),
 ( 4, 2, 2, 2, 2, 2, 2, 2, 2, 2, 2, 2, 2, 2, 2, 2, 2, 2, 2, 2, 2, 2, 2, 2, 2, 2, 2, 2, 2, 2, 2, 2, 2, 2, 2, 2, 2, 2, 2, 2, 2, 2, 2, 2, 2, 2, 2, 2, 2, 2, 2, 2, 2, 2, 2, 2, 2, 2, 2, 2, 2, 2, 2, 2, 2, 2, 2, 2, 2, 2, 2, 2, 2, 2, 2, 2, 2, 2, 2, 2, 2, 4 ),
 ( 0.000000000000000000, 1.000000000000000000 ),
 ( 0.0002080168337970193793, 0.0004025046291346534252, 0.0005969924244722874711, 0.0006942363221411045754, 0.0007914802198099215712, 0.0009859680151475555630, 0.001180455810485189772, 0.001277699708154006767, 0.001374943605822823763, 0.001472187503491640759, 0.001569431401160457755, 0.001763919196498091747, 0.001958406991835725738, 0.002055650889504542951, 0.002152894787173360164, 0.002347382582510994155, 0.002541870377848628147, 0.002639114275517445360, 0.002736358173186262139, 0.002930845968523896131, 0.003125333763861530122, 0.003222577661530346901, 0.003319821559199164114, 0.003417065456867981327, 0.003514309354536798539, 0.003708797149874432531, 0.003903284945212066523, 0.004097772740549700948, 0.004292260535887335374, 0.004486748331224968932, 0.004681236126562602490, 0.004875723921900236915, 0.005070211717237871341, 0.005264699512575504899, 0.005361943410244322111, 0.005459187307913138457, 0.005653675103250772882, 0.005848162898588407307, 0.005945406796257223653, 0.006042650693926040865, 0.006237138489263674423, 0.006431626284601308849, 0.006626114079938943274, 0.006820601875276577700, 0.007015089670614212125, 0.007112333568283028470, 0.007209577465951845683, 0.007404065261289479241, 0.007598553056627113667, 0.007695796954295930879, 0.007793040851964748092, 0.007890284749633564437, 0.007987528647302382517, 0.008182016442640016943, 0.008376504237977651368, 0.008473748135646467713, 0.008570992033315284059, 0.008765479828652918484, 0.008959967623990552910, 0.009057211521659369255, 0.009154455419328185600, 0.009348943214665820026, 0.009543431010003454451, 0.009640674907672272531, 0.009737918805341088876, 0.009835162703009905222, 0.009932406600678723302, 0.01012689439601635599, 0.01032138219135399042, 0.01041862608902280676, 0.01051586998669162484, 0.01071035778202925753, 0.01090484557736689196, 0.01109933337270452638, 0.01129382116804216081, 0.01148830896337979524, 0.01168279675871742793, 0.01187728455405506235, 0.01207177234939269678, 0.01226626014473032947, 0.01246074794006796389, 0.01265523573540559832 ),
 .UNSPECIFIED. ) ;
#3457 = CARTESIAN_POINT ( 'NONE',  ( -6.369687763352338550E-16, 186.8999999978150584, 9.500000000000001776 ) ) ;
#3458 = EDGE_CURVE ( 'NONE', #8784, #15622, #209, .T. ) ;
#3459 = CARTESIAN_POINT ( 'NONE',  ( -0.8817132232236292166, 228.8448810635624682, 8.679455557192847337 ) ) ;
#3460 = CARTESIAN_POINT ( 'NONE',  ( 5.649200442566231217, -2.675373855293995184, 17.38439807107078394 ) ) ;
#3461 = EDGE_CURVE ( 'NONE', #10282, #12193, #7572, .T. ) ;
#3462 = CARTESIAN_POINT ( 'NONE',  ( -0.7316483636516097899, 190.0789992933224255, 4.287069741549627722 ) ) ;
#3463 = VERTEX_POINT ( 'NONE', #14975 ) ;
#3464 = DIRECTION ( 'NONE',  ( -1.000000000000000000, 0.000000000000000000, 0.000000000000000000 ) ) ;
#3465 = CARTESIAN_POINT ( 'NONE',  ( 0.9999502950802738876, -5.916088184763872881, 11.63108149190010288 ) ) ;
#3467 = ORIENTED_EDGE ( 'NONE', *, *, #2786, .T. ) ;
#3466 = DIRECTION ( 'NONE',  ( 0.000000000000000000, 1.000000000000000000, 0.000000000000000000 ) ) ;
#3468 = CARTESIAN_POINT ( 'NONE',  ( 3.158296126777893953, -5.394094919772051355, 31.79887838423339019 ) ) ;
#3469 = CARTESIAN_POINT ( 'NONE',  ( 2.082642335314403343E-14, -6.250000000000000888, 32.00000000000000000 ) ) ;
#3470 = CARTESIAN_POINT ( 'NONE',  ( -2.500000000000000000, 0.000000000000000000, -0.5999999978150503122 ) ) ;
#3471 = CARTESIAN_POINT ( 'NONE',  ( 2.066987299999999639, 0.8561741729129456191, -0.4999999989075253337 ) ) ;
#3472 = CARTESIAN_POINT ( 'NONE',  ( -2.129935357778863558, 226.6102832534906213, 5.327017555938296844 ) ) ;
#3473 = CARTESIAN_POINT ( 'NONE',  ( -2.897581130414634077E-17, 22.00000000000000000, -9.750000000000003553 ) ) ;
#3474 = CARTESIAN_POINT ( 'NONE',  ( -2.500000000000000888, 187.5800000002184902, 8.035533905932737753 ) ) ;
#3475 = DIRECTION ( 'NONE',  ( 0.000000000000000000, 0.000000000000000000, 1.000000000000000000 ) ) ;
#3476 = CARTESIAN_POINT ( 'NONE',  ( -1.989902382949138460, 228.2815652486739282, 7.052567354366601649 ) ) ;
#3477 = EDGE_CURVE ( 'NONE', #6711, #260, #8935, .T. ) ;
#3478 = CARTESIAN_POINT ( 'NONE',  ( 0.000000000000000000, 184.0000000000000000, -2.999999999999997335 ) ) ;
#3479 = CARTESIAN_POINT ( 'NONE',  ( 2.066987299999999639, 2.531329380823229670E-16, 1.050000001092474822 ) ) ;
#3480 = FACE_OUTER_BOUND ( 'NONE', #11846, .T. ) ;
#3481 = ORIENTED_EDGE ( 'NONE', *, *, #2786, .F. ) ;
#3482 = CARTESIAN_POINT ( 'NONE',  ( -4.743384504624081899E-17, 186.8499999989074922, 4.933012699999999029 ) ) ;
#3483 = PRODUCT_DEFINITION_SHAPE ( 'NONE', 'NONE',  #15746 ) ;
#3484 = CARTESIAN_POINT ( 'NONE',  ( -1.461580736456473240, 186.1499999989075320, 5.538419263543526760 ) ) ;
#3485 = CARTESIAN_POINT ( 'NONE',  ( -2.841519077896137002, -5.566940434250017056, 11.76379616840804410 ) ) ;
#3486 =( REPRESENTATION_RELATIONSHIP ('NONE','NONE', #11191, #4596 ) REPRESENTATION_RELATIONSHIP_WITH_TRANSFORMATION ( #9968 )SHAPE_REPRESENTATION_RELATIONSHIP( ) );
#3487 = ORIENTED_EDGE ( 'NONE', *, *, #3658, .F. ) ;
#3488 = CARTESIAN_POINT ( 'NONE',  ( -3.735642931250969134, -4.696778275484520648, 4.025919472168996371 ) ) ;
#3489 = VECTOR ( 'NONE', #7082, 1000.000000000000000 ) ;
#3490 = CARTESIAN_POINT ( 'NONE',  ( 5.620786884546293827, -2.102685372472877567, 5.973585954366940065 ) ) ;
#3491 = CARTESIAN_POINT ( 'NONE',  ( 0.000000000000000000, 184.0000000000000000, -7.000000000000000000 ) ) ;
#3492 = FACE_OUTER_BOUND ( 'NONE', #11024, .T. ) ;
#3493 = CARTESIAN_POINT ( 'NONE',  ( -1.461580736456473240, 186.9499999989075150, 5.538419263543526760 ) ) ;
#3494 = CARTESIAN_POINT ( 'NONE',  ( 2.848727059635998149, -5.281416301279876713, 18.61442521571936837 ) ) ;
#3495 = CARTESIAN_POINT ( 'NONE',  ( -2.500000000000000000, 0.000000000000000000, 0.2000000021849497878 ) ) ;
#3496 = CARTESIAN_POINT ( 'NONE',  ( -5.570820891630784644, -2.833901239560364438, 4.737630265561251441 ) ) ;
#3497 = LINE ( 'NONE', #12088, #6196 ) ;
#3499 = CARTESIAN_POINT ( 'NONE',  ( -2.500000000000000000, 0.000000000000000000, 0.9000000000000000222 ) ) ;
#3498 = AXIS2_PLACEMENT_3D ( 'NONE', #2033, #6830, #11666 ) ;
#3500 = CARTESIAN_POINT ( 'NONE',  ( -5.859221468178978043, 2.178708437343151783, 10.52591457665827335 ) ) ;
#3501 = CARTESIAN_POINT ( 'NONE',  ( -0.02572782006998338561, 189.6977761910882805, 10.38959324765381709 ) ) ;
#3502 = AXIS2_PLACEMENT_3D ( 'NONE', #12204, #14265, #1226 ) ;
#3503 = ORIENTED_EDGE ( 'NONE', *, *, #4548, .T. ) ;
#3504 = EDGE_CURVE ( 'NONE', #13993, #10558, #702, .T. ) ;
#3505 = EDGE_LOOP ( 'NONE', ( #3953, #12586 ) ) ;
#3506 = EDGE_LOOP ( 'NONE', ( #12428, #1878 ) ) ;
#3507 = CARTESIAN_POINT ( 'NONE',  ( -3.922672396097124814, 4.541739265057643138, 12.37364704684421213 ) ) ;
#3508 = EDGE_CURVE ( 'NONE', #13977, #4648, #14592, .T. ) ;
#3509 = EDGE_LOOP ( 'NONE', ( #12911, #2411, #5686, #10267, #783, #4693 ) ) ;
#3510 = VECTOR ( 'NONE', #7057, 1000.000000000000114 ) ;
#3511 = CARTESIAN_POINT ( 'NONE',  ( 0.8561741729129451750, 2.066987299999999639, 1.800000001092475266 ) ) ;
#3512 = CARTESIAN_POINT ( 'NONE',  ( 1.000049560716553154, -5.916071405810146899, 4.869677990115314437 ) ) ;
#3513 = CARTESIAN_POINT ( 'NONE',  ( 5.649200442566148617, 2.675373855294168823, 31.61560192892921251 ) ) ;
#3514 = CARTESIAN_POINT ( 'NONE',  ( 2.066987300000000083, 187.6499999989075320, 7.000000000000000000 ) ) ;
#3515 = CARTESIAN_POINT ( 'NONE',  ( -1.035533905932738197, -2.500000000000000000, 1.056999999978150528 ) ) ;
#3516 = CARTESIAN_POINT ( 'NONE',  ( -5.317509234263959605, 2.779225709350992002, 31.00000000000000000 ) ) ;
#3517 = ITEM_DEFINED_TRANSFORMATION ( 'NONE', 'NONE', #760,  #14201 ) ;
#3518 = CARTESIAN_POINT ( 'NONE',  ( -1.265664690411614835E-16, 2.066987299999999639, 2.050000001092474822 ) ) ;
#3519 = CARTESIAN_POINT ( 'NONE',  ( 3.779681992289875669, -4.979315417303840974, 4.000049210157071045 ) ) ;
#3520 = CARTESIAN_POINT ( 'NONE',  ( -0.3933619333212962643, 226.3329841201265253, 4.509674143907711041 ) ) ;
#3521 = CARTESIAN_POINT ( 'NONE',  ( 6.106056299406729337, 1.336851112280767140, 5.798878384233397298 ) ) ;
#3522 = ORIENTED_EDGE ( 'NONE', *, *, #8143, .F. ) ;
#3523 = CIRCLE ( 'NONE', #4807, 3.118365096457675012 ) ;
#3524 = B_SPLINE_CURVE_WITH_KNOTS ( 'NONE', 3,
 ( #4826, #7215, #9438, #1077, #15644, #9518, #5783, #3620, #8326, #9682, #7294, #13165, #2264, #5938, #11971, #6978, #7135, #14439 ),
 .UNSPECIFIED., .F., .F.,
 ( 4, 2, 2, 2, 2, 2, 2, 2, 4 ),
 ( 0.000000000000000000, 0.0003914898357794968447, 0.0007829796715589936893, 0.001174469507338490480, 0.001565959343117988463, 0.001957449178897486229, 0.002348939014676983995, 0.002740428850456482195, 0.003131918686235979528 ),
 .UNSPECIFIED. ) ;
#3525 = VERTEX_POINT ( 'NONE', #14154 ) ;
#3526 = DIRECTION ( 'NONE',  ( -0.5877852522924685852, -0.8090169943749508930, 0.000000000000000000 ) ) ;
#3527 = ORIENTED_EDGE ( 'NONE', *, *, #12992, .F. ) ;
#3528 = EDGE_LOOP ( 'NONE', ( #12583, #5924 ) ) ;
#3529 = CARTESIAN_POINT ( 'NONE',  ( -6.155854678529470547, -1.081900940642134046, 30.49574050496988775 ) ) ;
#3530 = DIRECTION ( 'NONE',  ( -0.8660254037844385966, 0.5000000000000001110, 0.000000000000000000 ) ) ;
#3531 = CARTESIAN_POINT ( 'NONE',  ( -2.668367453516813370, -5.373994336898042512, 24.63236078583910427 ) ) ;
#3532 = CARTESIAN_POINT ( 'NONE',  ( 4.286401442266544848, -4.198423832313181059, 11.49999999999998224 ) ) ;
#3533 = CARTESIAN_POINT ( 'NONE',  ( 2.782468714962200274, 5.316055268221527186, 25.00389795015983196 ) ) ;
#3534 = COLOUR_RGB ( '', 0.09019608, 0.27058824, 0.51372549) ;
#3535 = CARTESIAN_POINT ( 'NONE',  ( 5.935543223013862502, -0.8771126767606430841, 31.00000000000000000 ) ) ;
#3536 = CARTESIAN_POINT ( 'NONE',  ( -4.152999119458038457, 4.671604476854301247, 12.30026515017674527 ) ) ;
#3537 = CARTESIAN_POINT ( 'NONE',  ( 5.843075991566567318, 1.368655265451115932, 30.12635295315577011 ) ) ;
#3538 = CARTESIAN_POINT ( 'NONE',  ( 0.2622916576878590589, -5.995491482261820160, 25.47384942646813499 ) ) ;
#3539 = DIRECTION ( 'NONE',  ( 1.000000000000000000, 0.000000000000000000, 0.000000000000000000 ) ) ;
#3540 = CARTESIAN_POINT ( 'NONE',  ( -1.035533905932739751, 186.8499999978150470, 9.500000000000003553 ) ) ;
#3541 = CARTESIAN_POINT ( 'NONE',  ( 0.6843230633849453071, 226.3504559366005537, 4.561183366923295068 ) ) ;
#3542 = FACE_OUTER_BOUND ( 'NONE', #14730, .T. ) ;
#3543 = CARTESIAN_POINT ( 'NONE',  ( 5.531757352715570342, 2.326874507723404761, 31.87380682714711355 ) ) ;
#3544 = VECTOR ( 'NONE', #7320, 1000.000000000000000 ) ;
#3545 = ORIENTED_EDGE ( 'NONE', *, *, #2829, .T. ) ;
#3546 = CARTESIAN_POINT ( 'NONE',  ( -4.142620314836359618, 4.341347824677524336, 4.385574784280628080 ) ) ;
#3547 = DIRECTION ( 'NONE',  ( 0.000000000000000000, 0.000000000000000000, 1.000000000000000000 ) ) ;
#3549 = VERTEX_POINT ( 'NONE', #3336 ) ;
#3548 = CARTESIAN_POINT ( 'NONE',  ( 5.903230462362981434, 1.077253041748728490, 25.11442521571936481 ) ) ;
#3550 = CARTESIAN_POINT ( 'NONE',  ( 4.069800786343840571, -4.744882212776791341, 31.87381964045071214 ) ) ;
#3551 = CARTESIAN_POINT ( 'NONE',  ( 7.490007020835692586, -2.433650805992223720, 31.00000000000000000 ) ) ;
#3552 = CARTESIAN_POINT ( 'NONE',  ( -3.107583187530477353, 5.133966411712655109, 10.62619317285287934 ) ) ;
#3553 = EDGE_CURVE ( 'NONE', #6574, #9005, #6937, .T. ) ;
#3554 = CARTESIAN_POINT ( 'NONE',  ( -0.8561741729129455081, 2.066987299999999639, 2.100000001092475088 ) ) ;
#3555 = CARTESIAN_POINT ( 'NONE',  ( -2.718436142382103071, 227.6979080801118300, 8.529473091820765518 ) ) ;
#3556 = COLOUR_RGB ( '', 0.40784314, 0.44705882, 0.49803922) ;
#3557 = CARTESIAN_POINT ( 'NONE',  ( -5.858813228503651160, 2.179803269293273615, 12.47377282875266324 ) ) ;
#3558 = CARTESIAN_POINT ( 'NONE',  ( -2.500000000000000444, 187.4800000002184959, 5.964466094067261359 ) ) ;
#3559 = CARTESIAN_POINT ( 'NONE',  ( -4.416837305303504380, 4.422286678979004293, 5.261902130840119263 ) ) ;
#3560 = CARTESIAN_POINT ( 'NONE',  ( -0.6404026449181154934, 227.6435107573390724, 5.209829591148105621 ) ) ;
#3561 = CARTESIAN_POINT ( 'NONE',  ( 0.4515139163396761357, 228.8949857255690290, 8.824160678851793449 ) ) ;
#3562 = CARTESIAN_POINT ( 'NONE',  ( 0.8561741729129465073, -2.066987299999999195, 0.1000000010924748939 ) ) ;
#3563 = CYLINDRICAL_SURFACE ( 'NONE', #5189, 2.500000000000000444 ) ;
#3564 = VERTEX_POINT ( 'NONE', #2137 ) ;
#3565 = CARTESIAN_POINT ( 'NONE',  ( -2.066987300000000527, 187.0499999989075093, 7.000000000000000000 ) ) ;
#3566 = CARTESIAN_POINT ( 'NONE',  ( 2.066987300000000971, 186.6999999989075150, 6.143825827087054492 ) ) ;
#3567 = CARTESIAN_POINT ( 'NONE',  ( -4.344762547369706240, -4.493114738039222011, 12.00308643866043568 ) ) ;
#3568 = ORIENTED_EDGE ( 'NONE', *, *, #3313, .F. ) ;
#3569 =( BOUNDED_SURFACE ( )  B_SPLINE_SURFACE ( 3, 2, ( 
 ( #233, #10976, #3883 ),
 ( #8756, #4941, #14642 ),
 ( #14478, #197, #13588 ),
 ( #3730, #8608, #7550 ),
 ( #10818, #15679, #7248 ),
 ( #12086, #1185, #6057 ),
 ( #10902, #1729, #12709 ),
 ( #1652, #7868, #383 ),
 ( #7784, #4282, #6374 ),
 ( #4044, #6526, #14952 ),
 ( #7705, #2856, #13665 ),
 ( #13749, #8915, #5334 ),
 ( #11514, #309, #15185 ),
 ( #13900, #3011, #461 ),
 ( #11286, #11208, #12475 ),
 ( #15030, #12554, #11361 ),
 ( #10177, #6604, #8835 ),
 ( #9147, #539, #8996 ),
 ( #11438, #4124, #1807 ),
 ( #12630, #13823, #2936 ),
 ( #5170, #5253, #6681 ),
 ( #5408, #13982, #2778 ),
 ( #10100, #3088, #12781 ),
 ( #10023, #10255, #9074 ),
 ( #7631, #15107, #4205 ),
 ( #615, #5487, #10331 ),
 ( #3961, #7941, #14871 ),
 ( #1576, #6454, #927 ),
 ( #8104, #6991, #5719 ),
 ( #10411, #14133, #8343 ),
 ( #15260, #11591, #11750 ),
 ( #691, #3238, #4681 ),
 ( #11820, #15579, #13098 ),
 ( #1963, #9222, #12942 ) ),
 .UNSPECIFIED., .F., .F., .F. ) 
 B_SPLINE_SURFACE_WITH_KNOTS ( ( 4, 2, 2, 2, 2, 2, 2, 2, 2, 2, 2, 2, 2, 2, 2, 2, 4 ),
 ( 3, 3 ),
 ( 0.000000000000000000, 0.0004059453939305676402, 0.0008118907878611352803, 0.001217836181791702920, 0.001623781575722270561, 0.002029726969652837984, 0.002435672363583405841, 0.002841617757513973698, 0.003247563151444541121, 0.003653508545375108545, 0.004059453939305675968, 0.004465399333236244259, 0.004871344727166811682, 0.005277290121097379105, 0.005683235515027947396, 0.006089180908958514819, 0.006495126302889082243 ),
 ( 0.000000000000000000, 1.000000000000000000 ),
 .UNSPECIFIED. ) 
 GEOMETRIC_REPRESENTATION_ITEM ( )  RATIONAL_B_SPLINE_SURFACE ( (
 ( 1.000000000000000000, 0.8248771365966364177, 1.000000000000000000),
 ( 1.000000000000000000, 0.8247993752883225893, 1.000000000000000000),
 ( 1.000000000000000000, 0.8250334644212878876, 1.000000000000000000),
 ( 1.000000000000000000, 0.8260937318508657645, 1.000000000000000000),
 ( 1.000000000000000000, 0.8269351727486546899, 1.000000000000000000),
 ( 1.000000000000000000, 0.8291161194214680119, 1.000000000000000000),
 ( 1.000000000000000000, 0.8304526363639401776, 1.000000000000000000),
 ( 1.000000000000000000, 0.8335574816758006822, 1.000000000000000000),
 ( 1.000000000000000000, 0.8353047682308820665, 1.000000000000000000),
 ( 1.000000000000000000, 0.8389997731991114538, 1.000000000000000000),
 ( 1.000000000000000000, 0.8409810165338121868, 1.000000000000000000),
 ( 1.000000000000000000, 0.8449567606309243972, 1.000000000000000000),
 ( 1.000000000000000000, 0.8469382525847787280, 1.000000000000000000),
 ( 1.000000000000000000, 0.8507236134161916263, 1.000000000000000000),
 ( 1.000000000000000000, 0.8525331645253796387, 1.000000000000000000),
 ( 1.000000000000000000, 0.8556292709850843448, 1.000000000000000000),
 ( 1.000000000000000000, 0.8569340980096278315, 1.000000000000000000),
 ( 1.000000000000000000, 0.8588235378423549893, 1.000000000000000000),
 ( 1.000000000000000000, 0.8593913334868529263, 1.000000000000000000),
 ( 1.000000000000000000, 0.8595838334664910318, 1.000000000000000000),
 ( 1.000000000000000000, 0.8592170625035302489, 1.000000000000000000),
 ( 1.000000000000000000, 0.8574834265527571109, 1.000000000000000000),
 ( 1.000000000000000000, 0.8561196021166810333, 1.000000000000000000),
 ( 1.000000000000000000, 0.8526284468138234374, 1.000000000000000000),
 ( 1.000000000000000000, 0.8504944293460048321, 1.000000000000000000),
 ( 1.000000000000000000, 0.8457235101200186733, 1.000000000000000000),
 ( 1.000000000000000000, 0.8431479293774302164, 1.000000000000000000),
 ( 1.000000000000000000, 0.8381225573515114213, 1.000000000000000000),
 ( 1.000000000000000000, 0.8356411947703757948, 1.000000000000000000),
 ( 1.000000000000000000, 0.8312972710846878721, 1.000000000000000000),
 ( 1.000000000000000000, 0.8294811344191250768, 1.000000000000000000),
 ( 1.000000000000000000, 0.8268651351247819914, 1.000000000000000000),
 ( 1.000000000000000000, 0.8260641663560207570, 1.000000000000000000),
 ( 1.000000000000000000, 0.8259116551296904474, 1.000000000000000000) ) ) 
 REPRESENTATION_ITEM ( '' )  SURFACE ( )  );
#3570 = EDGE_CURVE ( 'NONE', #4648, #13977, #15179, .T. ) ;
#3571 = LINE ( 'NONE', #10971, #4513 ) ;
#3572 = CARTESIAN_POINT ( 'NONE',  ( 0.8730628416138148662, 6.188929913094951551, 10.99504929893119609 ) ) ;
#3573 = CARTESIAN_POINT ( 'NONE',  ( 1.461580736456473240, 186.7499999989075263, 5.538419263543526760 ) ) ;
#3574 = PLANE ( 'NONE',  #11992 ) ;
#3575 = CARTESIAN_POINT ( 'NONE',  ( 4.592425496802573972E-16, -2.500000000000000000, -1.999999997815050001 ) ) ;
#3576 = CARTESIAN_POINT ( 'NONE',  ( 2.082642335314403343E-14, -6.000000000000000888, 32.00000000000000000 ) ) ;
#3577 = DIRECTION ( 'NONE',  ( -1.000000000000000000, 0.000000000000000000, 0.000000000000000000 ) ) ;
#3578 = CARTESIAN_POINT ( 'NONE',  ( -1.035533905932738197, -2.500000000000000000, 1.050000000000000044 ) ) ;
#3579 = DIRECTION ( 'NONE',  ( -0.000000000000000000, 1.000000000000000000, -0.000000000000000000 ) ) ;
#3580 =( BOUNDED_CURVE ( )  B_SPLINE_CURVE ( 2, ( #7231, #12069, #12379, #8739, #3866, #1636, #8665, #7456, #11557 ),
 .UNSPECIFIED., .F., .F. ) 
 B_SPLINE_CURVE_WITH_KNOTS ( ( 3, 2, 2, 2, 3 ),
 ( 0.5000000000000000000, 0.5178571428571429047, 0.5357142857142856984, 0.5535714285714286031, 0.5714285714285713969 ),
 .UNSPECIFIED. ) 
 CURVE ( )  GEOMETRIC_REPRESENTATION_ITEM ( )  RATIONAL_B_SPLINE_CURVE ( ( 1.000000000000000000, 0.9238795325112867385, 1.000000000000000000, 0.9238795325112867385, 1.000000000000000000, 0.9238795325112867385, 1.000000000000000000, 0.9238795325112867385, 1.000000000000000000 ) ) 
 REPRESENTATION_ITEM ( '' )  );
#3581 = CARTESIAN_POINT ( 'NONE',  ( -1.767766952966369320, 187.5000000000000000, 5.232233047033630235 ) ) ;
#3582 = EDGE_LOOP ( 'NONE', ( #15288, #2852, #6086, #12405 ) ) ;
#3583 = EDGE_CURVE ( 'NONE', #7332, #7142, #13820, .T. ) ;
#3584 = ORIENTED_EDGE ( 'NONE', *, *, #1627, .F. ) ;
#3585 = EDGE_LOOP ( 'NONE', ( #9691, #5379, #12917, #11080 ) ) ;
#3586 = CARTESIAN_POINT ( 'NONE',  ( -4.005361199355045088, 4.468319061418729810, 12.30022217383878846 ) ) ;
#3587 = ORIENTED_EDGE ( 'NONE', *, *, #7892, .T. ) ;
#3588 = CARTESIAN_POINT ( 'NONE',  ( -1.767766952966369098, 1.767766952966369098, -1.499999997815050223 ) ) ;
#3589 = FACE_BOUND ( 'NONE', #14008, .T. ) ;
#3590 = CARTESIAN_POINT ( 'NONE',  ( 5.770288754215095572, 2.404361317820031374, 31.87381964045071925 ) ) ;
#3591 = CARTESIAN_POINT ( 'NONE',  ( -2.066987300000000527, 188.8499999989074922, 7.000000000000000000 ) ) ;
#3592 = ADVANCED_FACE ( 'NONE', ( #15441 ), #4619, .F. ) ;
#3593 = CARTESIAN_POINT ( 'NONE',  ( 2.500000000000000444, 1.035533905932737975, -1.843000000021850049 ) ) ;
#3594 = DIRECTION ( 'NONE',  ( -0.000000000000000000, 1.000000000000000000, -0.000000000000000000 ) ) ;
#3595 = CARTESIAN_POINT ( 'NONE',  ( 2.066987300000000083, -0.8561741729129449530, 1.800000001092475266 ) ) ;
#3596 = CYLINDRICAL_SURFACE ( 'NONE', #15727, 2.500000000000000444 ) ;
#3597 = CARTESIAN_POINT ( 'NONE',  ( -2.960186505457850892, 227.4470585832885661, 7.791309201570119747 ) ) ;
#3598 = CARTESIAN_POINT ( 'NONE',  ( 2.817313151351047207, 5.579000502529503080, 11.49999999999998224 ) ) ;
#3599 = ORIENTED_EDGE ( 'NONE', *, *, #2498, .T. ) ;
#3600 = VECTOR ( 'NONE', #13706, 1000.000000000000000 ) ;
#3601 = EDGE_LOOP ( 'NONE', ( #11081, #180, #8706, #9195 ) ) ;
#3602 = CYLINDRICAL_SURFACE ( 'NONE', #13654, 2.500000000000000000 ) ;
#3603 = VERTEX_POINT ( 'NONE', #7010 ) ;
#3604 = VERTEX_POINT ( 'NONE', #15363 ) ;
#3605 = CARTESIAN_POINT ( 'NONE',  ( -5.858813228503603199, 2.179803269293398404, 25.47377282875267923 ) ) ;
#3606 = CARTESIAN_POINT ( 'NONE',  ( -4.291255145204137200, -4.544933371694618529, 23.88603820591928084 ) ) ;
#3607 = CARTESIAN_POINT ( 'NONE',  ( 6.780834061396424457E-14, 6.250000000000000888, 10.49999999999998224 ) ) ;
#3608 = CARTESIAN_POINT ( 'NONE',  ( -6.155854678529483870, 1.081900940642043452, 31.50425949503011225 ) ) ;
#3609 = CARTESIAN_POINT ( 'NONE',  ( 0.9999196734183355417, 5.916093360767503917, 11.36725955955069622 ) ) ;
#3610 = DIRECTION ( 'NONE',  ( 0.000000000000000000, 1.000000000000000000, 0.000000000000000000 ) ) ;
#3611 = ADVANCED_FACE ( 'NONE', ( #9391 ), #14303, .F. ) ;
#3612 = AXIS2_PLACEMENT_3D ( 'NONE', #1200, #15, #4877 ) ;
#3613 = CARTESIAN_POINT ( 'NONE',  ( -2.841041022017453344, 5.567186575787228087, 11.76225281721714566 ) ) ;
#3614 = CARTESIAN_POINT ( 'NONE',  ( 5.375886393124347684, 2.665038680141360139, 30.49560239355787417 ) ) ;
#3615 = CARTESIAN_POINT ( 'NONE',  ( 5.935543223013849179, 0.8771126767607271280, 31.00000000000000000 ) ) ;
#3616 = CARTESIAN_POINT ( 'NONE',  ( 0.000000000000000000, 144.0000000000000000, 0.000000000000000000 ) ) ;
#3617 = PRODUCT_DEFINITION_SHAPE ( 'NONE', 'NONE',  #15731 ) ;
#3618 = CARTESIAN_POINT ( 'NONE',  ( 1.767766952966368432, 188.5999999978150470, 8.767766952966368876 ) ) ;
#3619 = CARTESIAN_POINT ( 'NONE',  ( 1.751153496549405775, 226.5057898163625794, 5.019064844972819017 ) ) ;
#3620 = CARTESIAN_POINT ( 'NONE',  ( 3.736691294293418508, 4.695920479336378683, 31.97358595436693918 ) ) ;
#3621 = CARTESIAN_POINT ( 'NONE',  ( 5.867109477881222723, 1.259218163101011534, 31.79888242247940511 ) ) ;
#3622 = CIRCLE ( 'NONE', #14551, 20.00000000000000000 ) ;
#3623 = ORIENTED_EDGE ( 'NONE', *, *, #9073, .F. ) ;
#3624 = CARTESIAN_POINT ( 'NONE',  ( -2.668367453516709009, 5.373994336898094915, 4.867639214160893957 ) ) ;
#3625 = CARTESIAN_POINT ( 'NONE',  ( -0.2638277032948134759, -5.995407492418042494, 12.47332055281516716 ) ) ;
#3627 = ORIENTED_EDGE ( 'NONE', *, *, #7831, .T. ) ;
#3626 = CARTESIAN_POINT ( 'NONE',  ( 5.935543223013877601, 0.8771126767605438301, 24.63061695532138629 ) ) ;
#3628 = CARTESIAN_POINT ( 'NONE',  ( 3.566234721238137784, -5.134387337253762063, 31.99991741810289625 ) ) ;
#3629 = DIRECTION ( 'NONE',  ( 0.000000000000000000, -1.000000000000000000, 0.000000000000000000 ) ) ;
#3630 = CARTESIAN_POINT ( 'NONE',  ( 4.435347140100866170, 4.403429997944679819, 24.49999999999999289 ) ) ;
#3631 = CARTESIAN_POINT ( 'NONE',  ( 2.066987300000000083, -0.8561741729129449530, 1.800000001092475266 ) ) ;
#3632 = CARTESIAN_POINT ( 'NONE',  ( -4.344762547369864336, 4.493114738039070133, 23.99691356133952169 ) ) ;
#3633 = AXIS2_PLACEMENT_3D ( 'NONE', #15287, #12965, #7093 ) ;
#3634 = CARTESIAN_POINT ( 'NONE',  ( 0.8499999999999896527, 0.4000000000000062395, 2.749999999999994227 ) ) ;
#3635 = CARTESIAN_POINT ( 'NONE',  ( 2.500000000000000000, 187.8800000002185016, 8.035533905932739529 ) ) ;
#3636 = CARTESIAN_POINT ( 'NONE',  ( -4.344502777243558711, 4.493369211529237184, 5.503892131249680908 ) ) ;
#3637 = CARTESIAN_POINT ( 'NONE',  ( 1.724621985266778568, 228.5864789591000488, 7.933175541215780946 ) ) ;
#3638 = CARTESIAN_POINT ( 'NONE',  ( -1.461580736456472795, 1.461580736456472795, 1.350000001092474644 ) ) ;
#3639 = CARTESIAN_POINT ( 'NONE',  ( 5.984377695197246716, 1.807429553002209976, 16.99995093123465750 ) ) ;
#3640 = ORIENTED_EDGE ( 'NONE', *, *, #5939, .F. ) ;
#3641 = CARTESIAN_POINT ( 'NONE',  ( -2.066987300000001859, 188.6999999989075150, 7.856174172912944620 ) ) ;
#3642 = CARTESIAN_POINT ( 'NONE',  ( -1.461580736456473684, 185.5499999989075093, 8.461580736456474128 ) ) ;
#3643 = CARTESIAN_POINT ( 'NONE',  ( -2.817313151351169775, -5.579000502529442684, 11.49999999999998224 ) ) ;
#3644 = VERTEX_POINT ( 'NONE', #15601 ) ;
#3645 = AXIS2_PLACEMENT_3D ( 'NONE', #3491, #2295, #147 ) ;
#3646 = FACE_OUTER_BOUND ( 'NONE', #5498, .T. ) ;
#3647 = CARTESIAN_POINT ( 'NONE',  ( 0.9999505860955437697, -6.169489349035773174, 24.63105903165811839 ) ) ;
#3648 = CARTESIAN_POINT ( 'NONE',  ( 5.858736126997158955, -2.179962889276996663, 31.97359571723301741 ) ) ;
#3649 = CARTESIAN_POINT ( 'NONE',  ( 13.50000000000000000, 2.000000000000000000, 1.999999999999998668 ) ) ;
#3650 = CARTESIAN_POINT ( 'NONE',  ( -1.649561345686224145, 189.0000000000000000, 8.881879043882671354 ) ) ;
#3651 = CARTESIAN_POINT ( 'NONE',  ( 2.999999999999999556, -1.732050807568877859, -5.500000000000000000 ) ) ;
#3652 = CARTESIAN_POINT ( 'NONE',  ( 1.767766952966368654, 1.767766952966369098, -2.499999997815050445 ) ) ;
#3653 = DIRECTION ( 'NONE',  ( -6.123233995736766036E-17, 1.000000000000000000, 0.000000000000000000 ) ) ;
#3654 = CARTESIAN_POINT ( 'NONE',  ( 5.867109477881251145, -1.259218163100882970, 10.70111757752057002 ) ) ;
#3655 = CARTESIAN_POINT ( 'NONE',  ( -3.781065399486017053, 4.978303713186439161, 30.00008258189711441 ) ) ;
#3656 = CARTESIAN_POINT ( 'NONE',  ( -5.903843691985231956, 2.055287728870642816, 10.49995093123465395 ) ) ;
#3657 = CARTESIAN_POINT ( 'NONE',  ( -5.408775798201197027, 2.598833957129591532, 30.38602261056917442 ) ) ;
#3658 = EDGE_CURVE ( 'NONE', #12135, #14543, #7170, .T. ) ;
#3659 = ORIENTED_EDGE ( 'NONE', *, *, #9996, .F. ) ;
#3660 = SHAPE_REPRESENTATION ( 'connector', ( #14201 ), #13708 ) ;
#3661 = ADVANCED_FACE ( 'NONE', ( #3185 ), #6859, .F. ) ;
#3662 = ORIENTED_EDGE ( 'NONE', *, *, #14129, .T. ) ;
#3663 = ORIENTED_EDGE ( 'NONE', *, *, #9140, .T. ) ;
#3664 = B_SPLINE_CURVE_WITH_KNOTS ( 'NONE', 3,
 ( #11770, #7172, #14394, #8206, #7013, #14481, #10583, #4621, #13042, #9556, #12010, #8285, #15444, #8450, #1114, #797, #1032, #4784 ),
 .UNSPECIFIED., .F., .F.,
 ( 4, 2, 2, 2, 2, 2, 2, 2, 4 ),
 ( 0.000000000000000000, 0.0003914362731607599595, 0.0007828725463215199191, 0.001174308819482279987, 0.001565745092643039838, 0.001957181365803799689, 0.002348617638964559974, 0.002740053912125319825, 0.003131490185286079676 ),
 .UNSPECIFIED. ) ;
#3665 = CARTESIAN_POINT ( 'NONE',  ( -2.668367453516892418, 5.373994336898001656, 24.49999999999999289 ) ) ;
#3666 = VERTEX_POINT ( 'NONE', #6058 ) ;
#3667 = CARTESIAN_POINT ( 'NONE',  ( -1.767766952966369098, 1.767766952966369098, -2.299999997815050712 ) ) ;
#3668 = CARTESIAN_POINT ( 'NONE',  ( -6.176542424588095770, -0.9554180641287001174, 11.49999999999998224 ) ) ;
#3669 = CARTESIAN_POINT ( 'NONE',  ( 1.035533905932737531, 2.500000000000000444, -0.1499999999999999944 ) ) ;
#3670 = CARTESIAN_POINT ( 'NONE',  ( -1.461580736456473462, 187.3499999989075206, 8.461580736456472351 ) ) ;
#3671 = CARTESIAN_POINT ( 'NONE',  ( -2.500000000000000000, -0.4783542904563624076, 2.523096988312782063 ) ) ;
#3672 = AXIS2_PLACEMENT_3D ( 'NONE', #5276, #3111, #9168 ) ;
#3673 = DIRECTION ( 'NONE',  ( 0.000000000000000000, -1.000000000000000000, 0.000000000000000000 ) ) ;
#3674 = CARTESIAN_POINT ( 'NONE',  ( 3.011899281037468068, 5.190111395030246655, 5.800222173838807116 ) ) ;
#3675 = CARTESIAN_POINT ( 'NONE',  ( -2.066987299999999639, 0.8561741729129452860, -2.799999998907525267 ) ) ;
#3676 = CARTESIAN_POINT ( 'NONE',  ( -2.500000000000000000, 0.000000000000000000, -2.300000000000000266 ) ) ;
#3677 = CARTESIAN_POINT ( 'NONE',  ( -2.922039326512111401, 227.0704416020563201, 6.682560001249291837 ) ) ;
#3678 = DIRECTION ( 'NONE',  ( 0.000000000000000000, 0.000000000000000000, -1.000000000000000000 ) ) ;
#3679 = EDGE_LOOP ( 'NONE', ( #15291, #14330, #9380, #3082 ) ) ;
#3680 = ORIENTED_EDGE ( 'NONE', *, *, #788, .F. ) ;
#3681 = ORIENTED_EDGE ( 'NONE', *, *, #1143, .T. ) ;
#3682 = ORIENTED_EDGE ( 'NONE', *, *, #6146, .T. ) ;
#3683 = CARTESIAN_POINT ( 'NONE',  ( 8.572527594031473190E-16, 2.000000000000000000, 7.000000000000000000 ) ) ;
#3684 = CLOSED_SHELL ( 'NONE', ( #14930, #14667, #12649, #1427, #8535, #1257, #1037, #550, #9243, #10383, #8764, #14579, #14863, #12972, #10318, #10276, #12271, #15514, #2935, #6306 ) ) ;
#3685 = FILL_AREA_STYLE_COLOUR ( '', #14474 ) ;
#3686 = CARTESIAN_POINT ( 'NONE',  ( 2.500000000000000444, 185.5999999999999943, 7.000000000000000000 ) ) ;
#3687 = CARTESIAN_POINT ( 'NONE',  ( 3.735808404765003754, -4.696639218303121588, 12.47398020122237661 ) ) ;
#3688 = DIRECTION ( 'NONE',  ( 1.000000000000000000, 6.123233995736603333E-17, 6.123233995738439900E-17 ) ) ;
#3689 = CARTESIAN_POINT ( 'NONE',  ( -4.196288036172415303, -4.288789315524868861, 12.00312048902375039 ) ) ;
#3690 = CARTESIAN_POINT ( 'NONE',  ( -3.459447313391887047, 5.206669755180961090, 10.52599901976669194 ) ) ;
#3691 = CARTESIAN_POINT ( 'NONE',  ( -2.500000000000000000, 0.000000000000000000, -2.300000000000000266 ) ) ;
#3692 = CARTESIAN_POINT ( 'NONE',  ( 6.768587589771821120E-14, 6.000000000000000888, 12.49999999999998401 ) ) ;
#3693 = CARTESIAN_POINT ( 'NONE',  ( 9.750000000000003553, 26.00000000000000355, 1.020968533498575461E-13 ) ) ;
#3694 = ADVANCED_FACE ( 'NONE', ( #9720 ), #13590, .T. ) ;
#3695 = CARTESIAN_POINT ( 'NONE',  ( 2.500000000000000444, 187.0499999978150640, 8.035533905932739529 ) ) ;
#3696 = CARTESIAN_POINT ( 'NONE',  ( 2.961265621965179395, 227.4473031124620377, 7.792030372366526514 ) ) ;
#3697 = CARTESIAN_POINT ( 'NONE',  ( 2.897581130414634077E-17, 19.99999999999999645, 9.750000000000003553 ) ) ;
#3698 = FACE_OUTER_BOUND ( 'NONE', #3509, .T. ) ;
#3699 = EDGE_CURVE ( 'NONE', #786, #4232, #1417, .T. ) ;
#3700 = EDGE_LOOP ( 'NONE', ( #7036, #3819, #7579, #12667 ) ) ;
#3701 = CARTESIAN_POINT ( 'NONE',  ( -5.330004929009583670, 2.755647751839406023, 11.76239891805594695 ) ) ;
#3702 = CARTESIAN_POINT ( 'NONE',  ( 6.780834053290958173E-14, -6.000000000000000888, 10.49999999999998224 ) ) ;
#3703 = CARTESIAN_POINT ( 'NONE',  ( -1.767766952966369765, 187.7000000000000171, 8.767766952966368876 ) ) ;
#3704 = CARTESIAN_POINT ( 'NONE',  ( 5.935543223013889147, -0.8771126767604601193, 24.49999999999999289 ) ) ;
#3705 = CARTESIAN_POINT ( 'NONE',  ( 0.9161293052571292117, 226.3710829030681566, 4.621973948928255638 ) ) ;
#3706 = VECTOR ( 'NONE', #435, 1000.000000000000000 ) ;
#3707 = FACE_OUTER_BOUND ( 'NONE', #8873, .T. ) ;
#3708 = CARTESIAN_POINT ( 'NONE',  ( -1.265664690411614835E-16, 2.066987299999999639, 0.4500000010924747329 ) ) ;
#3709 = CYLINDRICAL_SURFACE ( 'NONE', #12504, 1.499999999999999556 ) ;
#3710 = FILL_AREA_STYLE ('',( #11189 ) ) ;
#3711 = CARTESIAN_POINT ( 'NONE',  ( -0.1323408341374683050, -6.250000000000002665, 32.00000000000000711 ) ) ;
#3712 = CARTESIAN_POINT ( 'NONE',  ( -1.035533905932739751, 188.4800000002184959, 9.500000000000003553 ) ) ;
#3713 = FACE_BOUND ( 'NONE', #10752, .T. ) ;
#3714 = CARTESIAN_POINT ( 'NONE',  ( 1.886647494277889692, 228.0514830721454871, 6.388076905524764371 ) ) ;
#3715 = CARTESIAN_POINT ( 'NONE',  ( 0.8561741729129465073, -2.066987299999999195, 0.9000000010924746885 ) ) ;
#3716 = CARTESIAN_POINT ( 'NONE',  ( 5.725930890718397670, -2.506952462183888120, 25.29933148907577234 ) ) ;
#3717 = AXIS2_PLACEMENT_3D ( 'NONE', #7635, #6458, #313 ) ;
#3718 = ORIENTED_EDGE ( 'NONE', *, *, #1355, .F. ) ;
#3719 = CARTESIAN_POINT ( 'NONE',  ( -6.776263578034402713E-16, 188.8499999989074922, 9.066987300000000971 ) ) ;
#3720 = CARTESIAN_POINT ( 'NONE',  ( 2.066987300000000083, 184.9999999989074979, 7.856174172912946396 ) ) ;
#3721 = CARTESIAN_POINT ( 'NONE',  ( 8.250000000000003553, -1.019131563299854308E-13, 2.000000000000001776 ) ) ;
#3723 = VERTEX_POINT ( 'NONE', #15729 ) ;
#3722 = CARTESIAN_POINT ( 'NONE',  ( -2.066987300000000083, 185.6499999989075320, 7.000000000000000000 ) ) ;
#3724 = FILL_AREA_STYLE ('',( #5967 ) ) ;
#3725 = CARTESIAN_POINT ( 'NONE',  ( 5.866817325727508248, -1.260653813891976061, 5.800222173838807116 ) ) ;
#3726 = DIRECTION ( 'NONE',  ( 0.000000000000000000, 1.000000000000000000, 0.000000000000000000 ) ) ;
#3727 =( REPRESENTATION_RELATIONSHIP ('NONE','NONE', #11191, #3660 ) REPRESENTATION_RELATIONSHIP_WITH_TRANSFORMATION ( #3053 )SHAPE_REPRESENTATION_RELATIONSHIP( ) );
#3728 = CARTESIAN_POINT ( 'NONE',  ( 2.066987300000000083, 188.2999999989075093, 6.143825827087054492 ) ) ;
#3729 = CARTESIAN_POINT ( 'NONE',  ( 5.486982057989271411, -2.429327048029698233, 25.29931806258174376 ) ) ;
#3730 = CARTESIAN_POINT ( 'NONE',  ( 0.5022380393797636344, 188.9999999999267004, 9.452991704445535603 ) ) ;
#3731 = B_SPLINE_CURVE_WITH_KNOTS ( 'NONE', 3,
 ( #7377, #8422, #2358, #8733, #4836, #1243, #5070, #13491, #13335, #11030, #9922, #7302, #1162, #7226, #10793, #11868, #6031, #3630 ),
 .UNSPECIFIED., .F., .F.,
 ( 4, 2, 2, 2, 2, 2, 2, 2, 4 ),
 ( 0.003131486019301992895, 0.003522824630466699601, 0.003914163241631405873, 0.004305501852796113013, 0.004696840463960820153, 0.005088179075125526425, 0.005479517686290233565, 0.005870856297454941572, 0.006262194908619648712 ),
 .UNSPECIFIED. ) ;
#3732 = DIRECTION ( 'NONE',  ( 0.000000000000000000, -1.000000000000000000, 0.000000000000000000 ) ) ;
#3733 = CARTESIAN_POINT ( 'NONE',  ( 5.843075991566589522, -1.368655265451022451, 31.87364704684421923 ) ) ;
#3734 = CARTESIAN_POINT ( 'NONE',  ( -5.621278735166232110, 2.101423246382466026, 10.52591947216897594 ) ) ;
#3735 = DIRECTION ( 'NONE',  ( -0.000000000000000000, 1.000000000000000000, -0.000000000000000000 ) ) ;
#3736 = CARTESIAN_POINT ( 'NONE',  ( -5.375763363753467416, 2.665284979407501087, 30.49610204984016448 ) ) ;
#3737 = VERTEX_POINT ( 'NONE', #8530 ) ;
#3738 = ORIENTED_EDGE ( 'NONE', *, *, #5282, .T. ) ;
#3739 = VECTOR ( 'NONE', #8200, 1000.000000000000000 ) ;
#3740 = VERTEX_POINT ( 'NONE', #9794 ) ;
#3741 = DIRECTION ( 'NONE',  ( 0.000000000000000000, 0.000000000000000000, -1.000000000000000000 ) ) ;
#3742 = EDGE_LOOP ( 'NONE', ( #9098, #11954, #4252, #9782 ) ) ;
#3743 = CARTESIAN_POINT ( 'NONE',  ( -2.066987299999999195, -0.8561741729129466183, 0.5000000010924746663 ) ) ;
#3744 = DIRECTION ( 'NONE',  ( 0.8660254037844385966, -0.4999999999999999445, 0.000000000000000000 ) ) ;
#3745 = ORIENTED_EDGE ( 'NONE', *, *, #2981, .T. ) ;
#3746 = CARTESIAN_POINT ( 'NONE',  ( 5.558508435838200867, 2.857531096718914920, 31.13234125634169658 ) ) ;
#3747 = CARTESIAN_POINT ( 'NONE',  ( -1.461580736456473240, 185.7499999989074979, 8.461580736456472351 ) ) ;
#3748 = CARTESIAN_POINT ( 'NONE',  ( 1.767766952966368654, 1.767766952966369098, 0.6000000000000000888 ) ) ;
#3749 = EDGE_CURVE ( 'NONE', #15704, #1426, #15680, .T. ) ;
#3750 = CARTESIAN_POINT ( 'NONE',  ( 9.750000000000003553, -1.020968533498575335E-13, 0.000000000000000000 ) ) ;
#3751 = ITEM_DEFINED_TRANSFORMATION ( 'NONE', 'NONE', #6559,  #14201 ) ;
#3752 = CARTESIAN_POINT ( 'NONE',  ( 2.848235266351006434, 5.281699484015658363, 5.613977389430844234 ) ) ;
#3753 = CARTESIAN_POINT ( 'NONE',  ( -2.066987299999999639, 0.8561741729129452860, -1.199999998907525622 ) ) ;
#3754 = DIRECTION ( 'NONE',  ( -0.5877852522924685852, -0.8090169943749508930, 0.000000000000000000 ) ) ;
#3755 = CARTESIAN_POINT ( 'NONE',  ( -2.691043998642291157, 227.7164964219492163, 8.584158233643494285 ) ) ;
#3756 = ORIENTED_EDGE ( 'NONE', *, *, #11823, .T. ) ;
#3757 = EDGE_LOOP ( 'NONE', ( #6304, #1136, #14751, #12410 ) ) ;
#3758 = VECTOR ( 'NONE', #13065, 1000.000000000000000 ) ;
#3759 = ORIENTED_EDGE ( 'NONE', *, *, #10476, .F. ) ;
#3760 = CARTESIAN_POINT ( 'NONE',  ( 5.903230462362963671, -1.077253041748834406, 30.38557478428061742 ) ) ;
#3761 = CARTESIAN_POINT ( 'NONE',  ( 2.079732659162522257, 189.0000000000000284, 5.600772967838274496 ) ) ;
#3762 = AXIS2_PLACEMENT_3D ( 'NONE', #15415, #13017, #773 ) ;
#3763 = CARTESIAN_POINT ( 'NONE',  ( -0.9737778612005471013, -5.920671847850519143, 4.737363758846508510 ) ) ;
#3764 = CARTESIAN_POINT ( 'NONE',  ( -6.021167129161054454, -1.680051667990301922, 31.97359571723301741 ) ) ;
#3765 = EDGE_CURVE ( 'NONE', #15426, #7891, #1218, .T. ) ;
#3766 = CARTESIAN_POINT ( 'NONE',  ( -1.626303258728256651E-16, 189.0624999997268390, 4.608253174999999757 ) ) ;
#3767 = CARTESIAN_POINT ( 'NONE',  ( 5.000000000000000000, 6.123233995736766282E-16, 2.000000000000001776 ) ) ;
#3768 = CARTESIAN_POINT ( 'NONE',  ( -5.570820891630826388, 2.833901239560284502, 5.262369734438755664 ) ) ;
#3769 = CARTESIAN_POINT ( 'NONE',  ( 2.500000000000000000, 3.061616997868383141E-16, 2.100000000000000089 ) ) ;
#3770 = CARTESIAN_POINT ( 'NONE',  ( 2.500000000000000000, 188.0000000000000000, 7.000000000000000000 ) ) ;
#3771 = DIRECTION ( 'NONE',  ( -1.000000000000000000, 0.000000000000000000, -3.491481338843133355E-15 ) ) ;
#3772 = AXIS2_PLACEMENT_3D ( 'NONE', #4315, #3195, #11544 ) ;
#3773 = CARTESIAN_POINT ( 'NONE',  ( 1.767766952966368432, 189.3999999978150584, 8.767766952966368876 ) ) ;
#3774 = CARTESIAN_POINT ( 'NONE',  ( 1.586671692599169736, 226.4708623422775418, 4.916117818249839289 ) ) ;
#3775 = CARTESIAN_POINT ( 'NONE',  ( -1.507559010347591544, 189.0898762284225825, 9.781293306605691740 ) ) ;
#3776 = ORIENTED_EDGE ( 'NONE', *, *, #12447, .T. ) ;
#3777 = CARTESIAN_POINT ( 'NONE',  ( -4.143041610105339778, 4.340967609747004019, 5.613977389430842457 ) ) ;
#3778 = DIRECTION ( 'NONE',  ( 0.000000000000000000, 0.000000000000000000, 1.000000000000000000 ) ) ;
#3779 = AXIS2_PLACEMENT_3D ( 'NONE', #12757, #6659, #11490 ) ;
#3780 = DIRECTION ( 'NONE',  ( 0.000000000000000000, 0.000000000000000000, -1.000000000000000000 ) ) ;
#3781 = DIRECTION ( 'NONE',  ( 0.000000000000000000, 0.000000000000000000, 1.000000000000000000 ) ) ;
#3782 = CARTESIAN_POINT ( 'NONE',  ( 1.318933956306606925, 226.4213524663575754, 4.770181869611323400 ) ) ;
#3783 = LINE ( 'NONE', #10876, #4627 ) ;
#3784 = CARTESIAN_POINT ( 'NONE',  ( -1.265664690411614835E-16, 2.066987299999999639, -0.3499999989075254225 ) ) ;
#3785 = CARTESIAN_POINT ( 'NONE',  ( -4.435347140101089103, 4.403429997944455110, 31.00000000000000000 ) ) ;
#3786 = EDGE_CURVE ( 'NONE', #12193, #10282, #15197, .T. ) ;
#3787 = CARTESIAN_POINT ( 'NONE',  ( 0.000000000000000000, 0.000000000000000000, -2.500000000000000000 ) ) ;
#3788 = CARTESIAN_POINT ( 'NONE',  ( -1.035533905932737975, 187.3800000002185016, 4.500000000000000888 ) ) ;
#3789 = DIRECTION ( 'NONE',  ( 0.000000000000000000, -1.000000000000000000, 0.000000000000000000 ) ) ;
#3791 = CARTESIAN_POINT ( 'NONE',  ( 0.1297182620452491941, 228.9108343529357228, 8.869932418632497928 ) ) ;
#3790 = PRESENTATION_LAYER_ASSIGNMENT (  '', '', ( #3282 ) ) ;
#3792 = DIRECTION ( 'NONE',  ( -1.000000000000000000, 0.000000000000000000, 0.000000000000000000 ) ) ;
#3793 = AXIS2_PLACEMENT_3D ( 'NONE', #14383, #9233, #14067 ) ;
#3794 = CARTESIAN_POINT ( 'NONE',  ( 0.5042987395407951823, 5.979983180450074265, 31.87329304179976219 ) ) ;
#3795 = ORIENTED_EDGE ( 'NONE', *, *, #9036, .F. ) ;
#3796 = CARTESIAN_POINT ( 'NONE',  ( -0.8561741729129458411, -2.066987299999999195, 0.6000000010924746441 ) ) ;
#3797 = ADVANCED_FACE ( 'NONE', ( #6292 ), #13444, .T. ) ;
#3798 = CARTESIAN_POINT ( 'NONE',  ( -5.793705359219414319E-16, 187.2499999989075263, 9.066987300000000971 ) ) ;
#3799 = DIRECTION ( 'NONE',  ( 6.123233995736782060E-17, -1.000000000000000000, 0.000000000000000000 ) ) ;
#3801 = VERTEX_POINT ( 'NONE', #7249 ) ;
#3800 = CARTESIAN_POINT ( 'NONE',  ( -1.461580736456472795, 184.7499999989074979, 5.538419263543527649 ) ) ;
#3802 = B_SPLINE_CURVE_WITH_KNOTS ( 'NONE', 3,
 ( #5400, #13742, #2769, #452, #7776, #5324, #6444, #4116, #6364, #4032, #2609, #12623, #14862, #1720, #5161, #11277, #13815, #8987 ),
 .UNSPECIFIED., .F., .F.,
 ( 4, 2, 2, 2, 2, 2, 2, 2, 4 ),
 ( 0.000000000000000000, 0.0003914898357794965194, 0.0007829796715589930388, 0.001174469507338489612, 0.001565959343117986078, 0.001957449178897482760, 0.002348939014676979225, 0.002740428850456475690, 0.003131918686235972155 ),
 .UNSPECIFIED. ) ;
#3803 = DIRECTION ( 'NONE',  ( 0.000000000000000000, 0.000000000000000000, -1.000000000000000000 ) ) ;
#3804 = STYLED_ITEM ( 'NONE', ( #10469 ), #4039 ) ;
#3805 = DIRECTION ( 'NONE',  ( 1.000000000000000000, -3.326610055774637112E-18, -1.062480551894331163E-17 ) ) ;
#3806 = PRESENTATION_STYLE_ASSIGNMENT (( #7165 ) ) ;
#3807 = CARTESIAN_POINT ( 'NONE',  ( 5.999999999999999112, 227.2817795252328210, 4.165129161027028459 ) ) ;
#3808 = CARTESIAN_POINT ( 'NONE',  ( 2.066987300000000083, 189.0499999989075093, 7.000000000000000000 ) ) ;
#3809 = FACE_BOUND ( 'NONE', #5043, .T. ) ;
#3810 = DIRECTION ( 'NONE',  ( 0.000000000000000000, 1.000000000000000000, 0.000000000000000000 ) ) ;
#3811 = CARTESIAN_POINT ( 'NONE',  ( -0.2638277032948710410, -5.995407492418040718, 31.97332055281518848 ) ) ;
#3812 = CARTESIAN_POINT ( 'NONE',  ( 5.782895619916176955, -1.604017620858013915, 31.97408052783100985 ) ) ;
#3813 = CARTESIAN_POINT ( 'NONE',  ( -0.8730628416135957082, -6.188929913094981750, 17.49504929893117477 ) ) ;
#3814 = ADVANCED_FACE ( 'NONE', ( #13359 ), #7401, .F. ) ;
#3815 = LINE ( 'NONE', #13517, #14913 ) ;
#3816 = CARTESIAN_POINT ( 'NONE',  ( 3.633127580202104134, 4.776802569231184847, 23.49992038825523011 ) ) ;
#3817 = EDGE_LOOP ( 'NONE', ( #8785, #2038 ) ) ;
#3818 = CARTESIAN_POINT ( 'NONE',  ( 1.461580736456472351, 186.7499999989075263, 8.461580736456474128 ) ) ;
#3819 = ORIENTED_EDGE ( 'NONE', *, *, #10559, .F. ) ;
#3820 = ORIENTED_EDGE ( 'NONE', *, *, #1216, .F. ) ;
#3821 = FACE_OUTER_BOUND ( 'NONE', #3369, .T. ) ;
#3822 = ORIENTED_EDGE ( 'NONE', *, *, #2508, .F. ) ;
#3823 = CARTESIAN_POINT ( 'NONE',  ( -2.066987299999999639, 0.000000000000000000, -0.3499999989075254225 ) ) ;
#3824 = CARTESIAN_POINT ( 'NONE',  ( -6.081464507797611496, -1.446657058464287715, 12.37380055247394672 ) ) ;
#3825 = DIRECTION ( 'NONE',  ( 1.000000000000000000, 0.000000000000000000, 0.000000000000000000 ) ) ;
#3826 = CARTESIAN_POINT ( 'NONE',  ( 2.449293598294706513E-15, 2.000000000000000000, 20.00000000000000000 ) ) ;
#3827 = CARTESIAN_POINT ( 'NONE',  ( -1.530808498934191571E-16, 2.500000000000000000, 1.500000000000000000 ) ) ;
#3828 = CYLINDRICAL_SURFACE ( 'NONE', #13538, 1.000000000000000888 ) ;
#3829 = EDGE_CURVE ( 'NONE', #8784, #6636, #15711, .T. ) ;
#3830 = CARTESIAN_POINT ( 'NONE',  ( 4.286401442266578599, -4.198423832313147308, 31.13236078583911137 ) ) ;
#3831 = CARTESIAN_POINT ( 'NONE',  ( -2.066987299999999639, 0.000000000000000000, -2.749999998907525445 ) ) ;
#3832 = CARTESIAN_POINT ( 'NONE',  ( -5.615973259022341679, 2.743340227996126757, 30.49610786875030044 ) ) ;
#3833 = CARTESIAN_POINT ( 'NONE',  ( -1.501309217710235622, 226.4539600517547910, 4.866297710963618073 ) ) ;
#3834 = ORIENTED_EDGE ( 'NONE', *, *, #11087, .T. ) ;
#3835 = ORIENTED_EDGE ( 'NONE', *, *, #13288, .T. ) ;
#3836 = ORIENTED_EDGE ( 'NONE', *, *, #13705, .F. ) ;
#3837 = AXIS2_PLACEMENT_3D ( 'NONE', #2593, #12062, #49 ) ;
#3838 = CARTESIAN_POINT ( 'NONE',  ( 5.843318061569056532, -1.367618216965589717, 30.12696220972948424 ) ) ;
#3839 = CARTESIAN_POINT ( 'NONE',  ( 3.566234721238087158, 5.134387337253796701, 4.000082581897114409 ) ) ;
#3840 = CARTESIAN_POINT ( 'NONE',  ( 7.347881158177969135E-16, 6.250000000000000888, 4.000000000000004441 ) ) ;
#3841 = CARTESIAN_POINT ( 'NONE',  ( -3.420311045507865355, -4.931422832349278806, 19.00007961174475213 ) ) ;
#3842 = CARTESIAN_POINT ( 'NONE',  ( 0.6144377077730618364, 5.969178481556058458, 10.70033966857734775 ) ) ;
#3843 = CARTESIAN_POINT ( 'NONE',  ( -1.767766952966369542, 185.1999999978150697, 8.767766952966368876 ) ) ;
#3844 = DIRECTION ( 'NONE',  ( 0.8090169943749506709, -0.5877852522924686962, 0.000000000000000000 ) ) ;
#3845 = CARTESIAN_POINT ( 'NONE',  ( -4.435347140101121965, 4.403429997944421359, 11.36939309276498911 ) ) ;
#3846 = CARTESIAN_POINT ( 'NONE',  ( 0.6152055445548323398, -5.969096820685134475, 25.29904968670267351 ) ) ;
#3847 = DIRECTION ( 'NONE',  ( 0.000000000000000000, -1.000000000000000000, 0.000000000000000000 ) ) ;
#3848 = CARTESIAN_POINT ( 'NONE',  ( 1.767766952966368654, 186.2699999975965568, 8.767766952966368876 ) ) ;
#3849 = CARTESIAN_POINT ( 'NONE',  ( -0.7022813136239680620, 227.6507649362739585, 5.230780073663146013 ) ) ;
#3850 = CARTESIAN_POINT ( 'NONE',  ( 2.599042177021809508, 227.7726851971488315, 8.749463102108622437 ) ) ;
#3851 = EDGE_CURVE ( 'NONE', #15393, #11257, #6052, .T. ) ;
#3852 = CARTESIAN_POINT ( 'NONE',  ( -3.827021247335478803E-16, 2.500000000000000000, -2.500000000000000000 ) ) ;
#3853 = ORIENTED_EDGE ( 'NONE', *, *, #5899, .T. ) ;
#3854 = ADVANCED_FACE ( 'NONE', ( #12087 ), #11133, .F. ) ;
#3855 = CARTESIAN_POINT ( 'NONE',  ( -5.903057025253910517, 1.078199533779480745, 12.11561732698603855 ) ) ;
#3856 = CARTESIAN_POINT ( 'NONE',  ( -5.570722351696290708, 2.834100162821917124, 30.73809786915987630 ) ) ;
#3857 = LINE ( 'NONE', #206, #3706 ) ;
#3858 = CARTESIAN_POINT ( 'NONE',  ( 2.030576276931546336E-13, 6.000000000000000888, 25.49999999999999645 ) ) ;
#3859 = CIRCLE ( 'NONE', #5903, 12.50000000000000533 ) ;
#3860 = CARTESIAN_POINT ( 'NONE',  ( 2.878492383785107744, 227.5628096391837971, 8.132007509143102553 ) ) ;
#3861 = CARTESIAN_POINT ( 'NONE',  ( 7.490007020835686369, -2.433650805992243260, 5.000000000000004441 ) ) ;
#3862 = CARTESIAN_POINT ( 'NONE',  ( -0.8561741729129458411, -2.066987299999999195, -1.599999998907525534 ) ) ;
#3863 = DIRECTION ( 'NONE',  ( -0.5877852522924685852, -0.8090169943749507819, 0.000000000000000000 ) ) ;
#3864 = CARTESIAN_POINT ( 'NONE',  ( -0.9737725088282058739, -6.173885267451823644, 30.73735758726567013 ) ) ;
#3865 = CARTESIAN_POINT ( 'NONE',  ( 2.500000000000000444, 185.5999999999999943, 7.000000000000000000 ) ) ;
#3866 = CARTESIAN_POINT ( 'NONE',  ( 4.592425496802573972E-16, -2.500000000000000000, -0.5000000000000000000 ) ) ;
#3867 = CARTESIAN_POINT ( 'NONE',  ( 1.923823996436629047, 228.4292023995385250, 7.478951866735841669 ) ) ;
#3868 = CARTESIAN_POINT ( 'NONE',  ( 2.066987299999999639, 0.8561741729129456191, -1.299999998907525267 ) ) ;
#3869 = CARTESIAN_POINT ( 'NONE',  ( 4.592425496802573972E-16, -2.500000000000000000, -2.799999997815050268 ) ) ;
#3870 = B_SPLINE_CURVE_WITH_KNOTS ( 'NONE', 3,
 ( #6112, #9842, #7375, #5947, #11978, #3468, #1159, #14613, #3628, #13489, #7143, #3550, #1313, #6028, #4991, #10949, #13412, #4914 ),
 .UNSPECIFIED., .F., .F.,
 ( 4, 2, 2, 2, 2, 2, 2, 2, 4 ),
 ( 0.003131486019301987257, 0.003522824630466694397, 0.003914163241631401537, 0.004305501852796108676, 0.004696840463960815816, 0.005088179075125522956, 0.005479517686290230095, 0.005870856297454937235, 0.006262194908619644375 ),
 .UNSPECIFIED. ) ;
#3871 = CARTESIAN_POINT ( 'NONE',  ( 2.066987299999999639, 2.531329380823229670E-16, 0.8500000010924746441 ) ) ;
#3872 = CARTESIAN_POINT ( 'NONE',  ( 0.8561741729129458411, 188.8999999989074752, 9.066987300000000971 ) ) ;
#3873 = CARTESIAN_POINT ( 'NONE',  ( -5.621278735166176155, -2.101423246382613463, 18.97408052783099563 ) ) ;
#3875 = ORIENTED_EDGE ( 'NONE', *, *, #3786, .T. ) ;
#3874 = CARTESIAN_POINT ( 'NONE',  ( 0.8561741729129455081, 185.3999999989075889, 4.933012699999999029 ) ) ;
#3876 = CARTESIAN_POINT ( 'NONE',  ( 0.000000000000000000, 0.000000000000000000, 2.500000000000000000 ) ) ;
#3877 = CYLINDRICAL_SURFACE ( 'NONE', #12628, 2.500000000000000444 ) ;
#3878 = CIRCLE ( 'NONE', #10488, 1.500000000000000000 ) ;
#3879 = CARTESIAN_POINT ( 'NONE',  ( 2.930922878467467019, -5.520395124723577851, 17.49610786875028623 ) ) ;
#3880 = CARTESIAN_POINT ( 'NONE',  ( -5.999999999999999112, 215.7452399395091618, 13.29567785264566027 ) ) ;
#3881 = CARTESIAN_POINT ( 'NONE',  ( -0.8730628416136632097, -6.188929913094972868, 10.99504929893116767 ) ) ;
#3882 = FACE_BOUND ( 'NONE', #7908, .T. ) ;
#3883 = CARTESIAN_POINT ( 'NONE',  ( -0.07717340183324516989, 189.6978550888158850, 10.38866401756453328 ) ) ;
#3884 = DIRECTION ( 'NONE',  ( 0.000000000000000000, 0.000000000000000000, 1.000000000000000000 ) ) ;
#3885 = CARTESIAN_POINT ( 'NONE',  ( 2.843793502989464983, 189.8324628781118690, 8.306572263327813843 ) ) ;
#3886 = CARTESIAN_POINT ( 'NONE',  ( -0.5030929395818956040, -6.230885867001155987, 17.12600319116547709 ) ) ;
#3887 = CARTESIAN_POINT ( 'NONE',  ( -7.180990026460683850, -3.384707322287710873, 24.49999999999999289 ) ) ;
#3888 = CARTESIAN_POINT ( 'NONE',  ( -0.3303979037561528553, 189.0000000000000284, 4.516547480436640782 ) ) ;
#3889 = ORIENTED_EDGE ( 'NONE', *, *, #113, .T. ) ;
#3890 = CARTESIAN_POINT ( 'NONE',  ( 2.066987299999999639, 188.4999999989074979, 6.143825827087054492 ) ) ;
#3891 = ORIENTED_EDGE ( 'NONE', *, *, #2375, .F. ) ;
#3892 = DIRECTION ( 'NONE',  ( -0.9510565162951544194, 0.3090169943749447312, 0.000000000000000000 ) ) ;
#3893 = ORIENTED_EDGE ( 'NONE', *, *, #8071, .F. ) ;
#3894 = EDGE_CURVE ( 'NONE', #1040, #12333, #4010, .T. ) ;
#3895 = FACE_OUTER_BOUND ( 'NONE', #6208, .T. ) ;
#3896 = EDGE_LOOP ( 'NONE', ( #8438, #14161, #4789, #13602 ) ) ;
#3897 = CARTESIAN_POINT ( 'NONE',  ( 2.066987299999999639, 0.8561741729129456191, -1.499999998907525445 ) ) ;
#3898 = CARTESIAN_POINT ( 'NONE',  ( 5.558508435838253270, 2.857531096718811892, 18.13234125634167526 ) ) ;
#3899 = CARTESIAN_POINT ( 'NONE',  ( -2.696515973634777907, 189.9486803746651162, 5.919686589971288271 ) ) ;
#3900 = CYLINDRICAL_SURFACE ( 'NONE', #568, 1.000000000000000666 ) ;
#3901 = AXIS2_PLACEMENT_3D ( 'NONE', #10495, #934, #14062 ) ;
#3902 = CARTESIAN_POINT ( 'NONE',  ( -2.500000000000000000, -1.035533905932739307, -2.243000000021849516 ) ) ;
#3903 = CARTESIAN_POINT ( 'NONE',  ( -3.736532060718099402, 4.696070028785882755, 17.02622176056705783 ) ) ;
#3904 = CONTEXT_DEPENDENT_SHAPE_REPRESENTATION ( #7819, #1947 ) ;
#3905 = CARTESIAN_POINT ( 'NONE',  ( -6.176542424588072677, -0.9554180641288341214, 24.49999999999999289 ) ) ;
#3906 = CARTESIAN_POINT ( 'NONE',  ( 2.066987300000000083, -0.8561741729129449530, 0.2000000010924747329 ) ) ;
#3907 = CARTESIAN_POINT ( 'NONE',  ( 5.558508435838262152, -2.857531096718793240, 11.36765874365828743 ) ) ;
#3908 = CARTESIAN_POINT ( 'NONE',  ( -2.951760543192366804, 227.4626507460308744, 7.837199003427246069 ) ) ;
#3909 = ORIENTED_EDGE ( 'NONE', *, *, #9693, .F. ) ;
#3910 = ORIENTED_EDGE ( 'NONE', *, *, #12092, .T. ) ;
#3911 = ORIENTED_EDGE ( 'NONE', *, *, #13470, .F. ) ;
#3912 = CARTESIAN_POINT ( 'NONE',  ( 5.935543223013863390, -0.8771126767606431951, 30.86938304467861727 ) ) ;
#3913 = CARTESIAN_POINT ( 'NONE',  ( 0.4407554183254575597, 188.9999999999999716, 4.532388849764692473 ) ) ;
#3914 = VERTEX_POINT ( 'NONE', #8757 ) ;
#3915 = CARTESIAN_POINT ( 'NONE',  ( -1.000079958708137928, -5.916066267613700802, 5.131527388820333435 ) ) ;
#3916 = CARTESIAN_POINT ( 'NONE',  ( -3.923477796648590754, -4.541042560386415516, 18.87303779027050155 ) ) ;
#3917 = CARTESIAN_POINT ( 'NONE',  ( 4.069684453406231306, -4.744965295353614110, 23.62619944752604084 ) ) ;
#3918 = CARTESIAN_POINT ( 'NONE',  ( 2.500000000000000444, 187.8999999978150584, 7.000000000000000000 ) ) ;
#3919 = CARTESIAN_POINT ( 'NONE',  ( 0.000000000000000000, 186.4999999978150527, 4.500000000000000000 ) ) ;
#3920 = CARTESIAN_POINT ( 'NONE',  ( -2.500000000000000444, 185.2000000000000171, 7.000000000000000000 ) ) ;
#3921 = CARTESIAN_POINT ( 'NONE',  ( -4.435347140101121965, 4.403429997944421359, 11.49999999999998224 ) ) ;
#3922 = CARTESIAN_POINT ( 'NONE',  ( 0.9735856429314875271, -5.920699391844991943, 24.76285283906726065 ) ) ;
#3923 = CARTESIAN_POINT ( 'NONE',  ( -1.361387964035781121E-13, 146.0000000000000000, 9.750000000000003553 ) ) ;
#3924 = CARTESIAN_POINT ( 'NONE',  ( 2.500000000000000444, 186.3199999975965966, 8.035533905932739529 ) ) ;
#3925 = CARTESIAN_POINT ( 'NONE',  ( 0.3253281796544252868, 227.6173729869818771, 5.134342219554626219 ) ) ;
#3926 = CARTESIAN_POINT ( 'NONE',  ( -2.191791664054325572, 227.9495085101182781, 9.269582106420829248 ) ) ;
#3927 = AXIS2_PLACEMENT_3D ( 'NONE', #9474, #5977, #5663 ) ;
#3928 = CARTESIAN_POINT ( 'NONE',  ( -2.815864604846499919, 189.2275809052524664, 8.215757671725111067 ) ) ;
#3929 = VERTEX_POINT ( 'NONE', #10819 ) ;
#3930 = LINE ( 'NONE', #6424, #223 ) ;
#3931 = APPLICATION_CONTEXT ( 'automotive_design' ) ;
#3932 = DIRECTION ( 'NONE',  ( 0.5877852522924802425, -0.8090169943749422332, 0.000000000000000000 ) ) ;
#3933 = CARTESIAN_POINT ( 'NONE',  ( 6.768587589771821120E-14, -6.250000000000000888, 12.49999999999998401 ) ) ;
#3934 = CARTESIAN_POINT ( 'NONE',  ( 5.726049995854468833, 2.506679546901878552, 12.29954462468842991 ) ) ;
#3935 = CARTESIAN_POINT ( 'NONE',  ( 0.7710626327916485501, 228.2248363320221642, 10.07924096547705872 ) ) ;
#3936 = CARTESIAN_POINT ( 'NONE',  ( 4.435347140101010943, 4.403429997944536822, 5.132374107163055754 ) ) ;
#3937 = CARTESIAN_POINT ( 'NONE',  ( 2.066987299999999639, 2.531329380823229670E-16, -2.149999998907525356 ) ) ;
#3938 = CARTESIAN_POINT ( 'NONE',  ( 7.490007020835692586, -2.433650805992223720, 31.00000000000000000 ) ) ;
#3939 = EDGE_CURVE ( 'NONE', #5534, #11257, #1186, .T. ) ;
#3940 = DIRECTION ( 'NONE',  ( 0.8090169943749421222, 0.5877852522924802425, 0.000000000000000000 ) ) ;
#3941 = CARTESIAN_POINT ( 'NONE',  ( 2.500000000000000444, 184.8499999999999943, 5.964466094067262247 ) ) ;
#3942 = CARTESIAN_POINT ( 'NONE',  ( 4.592425496802573972E-16, -2.500000000000000000, -1.999999997815050001 ) ) ;
#3943 = EDGE_CURVE ( 'NONE', #15370, #7094, #13983, .T. ) ;
#3944 = CARTESIAN_POINT ( 'NONE',  ( -1.288813234857717038, 227.7638191499166851, 5.557287090853593625 ) ) ;
#3945 = CARTESIAN_POINT ( 'NONE',  ( -0.8561741729129455081, 2.066987299999999639, -1.099999998907525312 ) ) ;
#3946 = CARTESIAN_POINT ( 'NONE',  ( 5.770331821586490051, -2.404225004693387291, 25.37380055247395561 ) ) ;
#3947 = B_SPLINE_CURVE_WITH_KNOTS ( 'NONE', 3,
 ( #105, #13544, #5123, #11316, #9976, #415, #7581, #5047, #5285, #14752, #12430, #2886, #1530, #6405, #11237, #339, #5201, #10054 ),
 .UNSPECIFIED., .F., .F.,
 ( 4, 2, 2, 2, 2, 2, 2, 2, 4 ),
 ( 0.003131923598876997471, 0.003523316383094315246, 0.003914709167311632154, 0.004306101951528949930, 0.004697494735746267705, 0.005088887519963585480, 0.005480280304180903256, 0.005871673088398220164, 0.006263065872615537939 ),
 .UNSPECIFIED. ) ;
#3948 = CARTESIAN_POINT ( 'NONE',  ( 1.461580736456472573, 1.461580736456472795, 1.750000001092474999 ) ) ;
#3949 = CARTESIAN_POINT ( 'NONE',  ( 1.423015351387224570E-16, 184.1999999999999886, 4.500000000000000000 ) ) ;
#3950 = CARTESIAN_POINT ( 'NONE',  ( -5.842945980534627104, -1.369128644669050043, 18.87378430870261781 ) ) ;
#3951 = CIRCLE ( 'NONE', #15139, 6.250000000000000888 ) ;
#3953 = ORIENTED_EDGE ( 'NONE', *, *, #2105, .T. ) ;
#3952 = CARTESIAN_POINT ( 'NONE',  ( -0.8561741729129469514, 188.9999999989075263, 9.066987299999999195 ) ) ;
#3954 = CARTESIAN_POINT ( 'NONE',  ( -7.490007020835664164, -2.433650805992495503, 17.99999999999998934 ) ) ;
#3955 = ADVANCED_FACE ( 'NONE', ( #12398 ), #7785, .F. ) ;
#3956 = DIRECTION ( 'NONE',  ( -1.000000000000000000, 0.000000000000000000, 0.000000000000000000 ) ) ;
#3957 = CARTESIAN_POINT ( 'NONE',  ( 3.659182332138577465E-16, 227.2817795252328210, 4.165129161027028459 ) ) ;
#3958 = EDGE_CURVE ( 'NONE', #15527, #7039, #4519, .T. ) ;
#3959 = CARTESIAN_POINT ( 'NONE',  ( -1.968030457003884015, 189.0000000000000000, 8.558443299018994921 ) ) ;
#3960 = CARTESIAN_POINT ( 'NONE',  ( 4.195795028114952530, 4.289273350251397332, 17.49571079637979309 ) ) ;
#3961 = CARTESIAN_POINT ( 'NONE',  ( 1.727510648855079767, 189.0000000003634000, 5.183832296574240495 ) ) ;
#3962 = CARTESIAN_POINT ( 'NONE',  ( 0.000000000000000000, 0.000000000000000000, 0.000000000000000000 ) ) ;
#3963 = CARTESIAN_POINT ( 'NONE',  ( 2.046795664782080415, 190.0128272625842953, 5.019430763338620594 ) ) ;
#3964 = CARTESIAN_POINT ( 'NONE',  ( -4.435347140101088215, 4.403429997944455998, 30.86939309276502641 ) ) ;
#3965 = CYLINDRICAL_SURFACE ( 'NONE', #665, 1.000000000000000222 ) ;
#3966 = CYLINDRICAL_SURFACE ( 'NONE', #7713, 1.000000000000000888 ) ;
#3967 = ORIENTED_EDGE ( 'NONE', *, *, #13803, .F. ) ;
#3968 = CARTESIAN_POINT ( 'NONE',  ( 0.8561741729129458411, 188.2999999989075093, 9.066987299999999195 ) ) ;
#3969 = ORIENTED_EDGE ( 'NONE', *, *, #10127, .F. ) ;
#3970 = CARTESIAN_POINT ( 'NONE',  ( -5.746996058422734421, 1.729015645942056478, 25.50007961174475923 ) ) ;
#3971 = ORIENTED_EDGE ( 'NONE', *, *, #8593, .F. ) ;
#3972 = DIRECTION ( 'NONE',  ( 1.000000000000000000, 0.000000000000000000, 0.000000000000000000 ) ) ;
#3973 = CYLINDRICAL_SURFACE ( 'NONE', #15468, 2.500000000000000444 ) ;
#3974 = EDGE_LOOP ( 'NONE', ( #9767, #9319 ) ) ;
#3975 = CARTESIAN_POINT ( 'NONE',  ( 1.461580736456473018, -1.461580736456472573, -0.04999999890752549608 ) ) ;
#3976 = CARTESIAN_POINT ( 'NONE',  ( 1.767766952966368654, 1.767766952966369098, -1.800000000000000044 ) ) ;
#3977 = CARTESIAN_POINT ( 'NONE',  ( -0.7858668154420391794, 190.0775333035548158, 4.301934987860914106 ) ) ;
#3978 = DIRECTION ( 'NONE',  ( -0.000000000000000000, -1.000000000000000000, -0.000000000000000000 ) ) ;
#3979 = CARTESIAN_POINT ( 'NONE',  ( -1.767766952966369098, 1.767766952966369098, -1.600000000000000311 ) ) ;
#3980 = CARTESIAN_POINT ( 'NONE',  ( -7.490007020835684592, -2.433650805992431110, 11.49999999999998224 ) ) ;
#3981 = CARTESIAN_POINT ( 'NONE',  ( 3.735808404765050827, -4.696639218303082508, 31.97398020122238549 ) ) ;
#3982 = CARTESIAN_POINT ( 'NONE',  ( -0.8561741729129458411, -2.066987299999999195, 0.8000000010924747107 ) ) ;
#3983 = ADVANCED_FACE ( 'NONE', ( #15108 ), #1730, .F. ) ;
#3984 = CARTESIAN_POINT ( 'NONE',  ( 5.649200442566201019, -2.675373855294060910, 10.88439807107078572 ) ) ;
#3985 = CARTESIAN_POINT ( 'NONE',  ( -0.8738043859790617374, 6.188821459035881212, 31.50341560223747450 ) ) ;
#3986 = ORIENTED_EDGE ( 'NONE', *, *, #14352, .T. ) ;
#3987 = PRODUCT_RELATED_PRODUCT_CATEGORY ( 'part', '', ( #12844 ) ) ;
#3988 = ORIENTED_EDGE ( 'NONE', *, *, #2984, .T. ) ;
#3989 = EDGE_CURVE ( 'NONE', #4626, #9974, #616, .T. ) ;
#3990 = VERTEX_POINT ( 'NONE', #8916 ) ;
#3991 = DIRECTION ( 'NONE',  ( 0.000000000000000000, 0.000000000000000000, 1.000000000000000000 ) ) ;
#3992 = CARTESIAN_POINT ( 'NONE',  ( 1.530808498934191916E-15, 19.99999999999999645, -12.50000000000000355 ) ) ;
#3993 = ORIENTED_EDGE ( 'NONE', *, *, #10195, .F. ) ;
#3994 = AXIS2_PLACEMENT_3D ( 'NONE', #14367, #14534, #9848 ) ;
#3995 = CARTESIAN_POINT ( 'NONE',  ( 0.7988860301922214857, 6.199427171881336740, 4.384555805361944891 ) ) ;
#3996 = B_SPLINE_CURVE_WITH_KNOTS ( 'NONE', 3,
 ( #5142, #359, #15007, #5225, #8806, #4013, #8728, #1549, #9839, #4097, #6343, #8967, #12367, #13635, #433, #10072, #11180, #11336 ),
 .UNSPECIFIED., .F., .F.,
 ( 4, 2, 2, 2, 2, 2, 2, 2, 4 ),
 ( 0.000000000000000000, 0.0003914357524127463472, 0.0007828715048254926943, 0.001174307257238239042, 0.001565743009650985389, 0.001957178762063731953, 0.002348614514476478083, 0.002740050266889224213, 0.003131486019301970777 ),
 .UNSPECIFIED. ) ;
#3997 = CARTESIAN_POINT ( 'NONE',  ( 0.7993282387951309298, -5.947240459526506484, 31.61484358216957347 ) ) ;
#3998 = VECTOR ( 'NONE', #1180, 1000.000000000000000 ) ;
#3999 = CARTESIAN_POINT ( 'NONE',  ( -0.7993401192311065939, 6.199366368793671533, 18.61483246936565550 ) ) ;
#4000 = CARTESIAN_POINT ( 'NONE',  ( 0.1323408341374927855, 6.250000000000000888, 19.00000000000000711 ) ) ;
#4001 = CARTESIAN_POINT ( 'NONE',  ( 2.500000000000000444, 185.4499999978150981, 8.035533905932739529 ) ) ;
#4002 = SURFACE_STYLE_FILL_AREA ( #13711 ) ;
#4003 = CARTESIAN_POINT ( 'NONE',  ( -3.255013540813682660, 5.336859797930809890, 10.62618035954927898 ) ) ;
#4004 = DIRECTION ( 'NONE',  ( -0.000000000000000000, -1.000000000000000000, -0.000000000000000000 ) ) ;
#4005 =( NAMED_UNIT ( * ) PLANE_ANGLE_UNIT ( ) SI_UNIT ( $, .RADIAN. ) );
#4006 = CARTESIAN_POINT ( 'NONE',  ( -3.388131789017201356E-18, 186.5699999975965397, 4.500000000000000000 ) ) ;
#4007 = CARTESIAN_POINT ( 'NONE',  ( -1.361424426418679889, 228.7361946629245892, 8.365563033085530620 ) ) ;
#4008 = CARTESIAN_POINT ( 'NONE',  ( -1.942272232823049061, 226.5542875158922129, 5.161998670295230518 ) ) ;
#4009 = CIRCLE ( 'NONE', #8337, 6.000000000000000000 ) ;
#4010 = CIRCLE ( 'NONE', #12896, 1.499999999999999556 ) ;
#4011 = CARTESIAN_POINT ( 'NONE',  ( -2.665324589450957848, 189.8106497419773291, 8.736655013898124267 ) ) ;
#4012 = EDGE_LOOP ( 'NONE', ( #13617, #3294, #10826, #11850 ) ) ;
#4013 = CARTESIAN_POINT ( 'NONE',  ( -6.105925084677680914, 1.337450587213181441, 17.20066851092422411 ) ) ;
#4014 = CARTESIAN_POINT ( 'NONE',  ( 3.883716939929109380, -4.898343590941151682, 10.52640428276697548 ) ) ;
#4015 = DIRECTION ( 'NONE',  ( 1.000000000000000000, 0.000000000000000000, 0.000000000000000000 ) ) ;
#4016 = DIRECTION ( 'NONE',  ( 0.000000000000000000, 1.000000000000000000, 0.000000000000000000 ) ) ;
#4017 = CARTESIAN_POINT ( 'NONE',  ( 2.273809214555841951, 227.9194763741126906, 9.181262328259517602 ) ) ;
#4018 = CIRCLE ( 'NONE', #13431, 1.499999999999999556 ) ;
#4019 = CARTESIAN_POINT ( 'NONE',  ( 3.159612573729236651, 5.393342049074624001, 5.800265150176763029 ) ) ;
#4020 = CARTESIAN_POINT ( 'NONE',  ( 3.796994071234844259E-16, -2.066987299999999639, -1.549999998907525045 ) ) ;
#4021 = CARTESIAN_POINT ( 'NONE',  ( 2.782156709077406642, 5.316215864844050287, 4.496879510976234506 ) ) ;
#4022 = FILL_AREA_STYLE ('',( #5074 ) ) ;
#4023 = DIRECTION ( 'NONE',  ( 0.000000000000000000, 1.000000000000000000, 0.000000000000000000 ) ) ;
#4024 = CARTESIAN_POINT ( 'NONE',  ( 1.767766952966369098, 187.2999999999999829, 5.232233047033630235 ) ) ;
#4025 = FACE_BOUND ( 'NONE', #3019, .T. ) ;
#4026 = CARTESIAN_POINT ( 'NONE',  ( -1.238081232355301875, 227.7501834494555055, 5.517906410191214306 ) ) ;
#4027 = CYLINDRICAL_SURFACE ( 'NONE', #6528, 2.500000000000000444 ) ;
#4028 = CARTESIAN_POINT ( 'NONE',  ( -2.817313151351169775, -5.579000502529442684, 11.49999999999998224 ) ) ;
#4029 = CARTESIAN_POINT ( 'NONE',  ( -2.066987299999999639, 0.000000000000000000, 1.250000001092474777 ) ) ;
#4030 = CARTESIAN_POINT ( 'NONE',  ( 5.531796221294920990, 2.326749136277109109, 23.62621569129737509 ) ) ;
#4031 = CARTESIAN_POINT ( 'NONE',  ( -0.8561741729129472844, 188.7999999989075093, 9.066987300000000971 ) ) ;
#4032 = CARTESIAN_POINT ( 'NONE',  ( -3.632151824461173462, 4.777505256984529325, 19.00004932073311181 ) ) ;
#4033 = VECTOR ( 'NONE', #6400, 1000.000000000000114 ) ;
#4035 = VERTEX_POINT ( 'NONE', #13901 ) ;
#4034 = CARTESIAN_POINT ( 'NONE',  ( -2.066987300000000083, 186.3999999989075320, 6.143825827087054492 ) ) ;
#4036 = EDGE_CURVE ( 'NONE', #8231, #14335, #3012, .T. ) ;
#4037 = CARTESIAN_POINT ( 'NONE',  ( -3.779082820360704087, -4.979770177899243144, 16.99995093123465750 ) ) ;
#4038 = CARTESIAN_POINT ( 'NONE',  ( 5.935543223013860725, -0.8771126767606638452, 5.130649613488545313 ) ) ;
#4039 = ADVANCED_BREP_SHAPE_REPRESENTATION ( '', ( #15531, #14201 ), #10667 ) ;
#4040 = CARTESIAN_POINT ( 'NONE',  ( -5.935543223013861613, 0.8771126767606655106, 5.000000000000004441 ) ) ;
#4041 = DIRECTION ( 'NONE',  ( 1.000000000000000000, 0.000000000000000000, 0.000000000000000000 ) ) ;
#4042 =( GEOMETRIC_REPRESENTATION_CONTEXT ( 3 ) GLOBAL_UNCERTAINTY_ASSIGNED_CONTEXT ( ( #6173 ) ) GLOBAL_UNIT_ASSIGNED_CONTEXT ( ( #14055, #8020, #2196 ) ) REPRESENTATION_CONTEXT ( 'NONE', 'WORKASPACE' ) );
#4043 = CARTESIAN_POINT ( 'NONE',  ( 5.935543223013889147, -0.8771126767604600083, 24.63064961348855775 ) ) ;
#4044 = CARTESIAN_POINT ( 'NONE',  ( 1.644293605570781969, 188.9999999996334168, 8.888752494527455639 ) ) ;
#4045 = CARTESIAN_POINT ( 'NONE',  ( 0.02104286312898811379, -0.3999999999999941380, -2.514165122916821371 ) ) ;
#4046 = CARTESIAN_POINT ( 'NONE',  ( 4.005785023174528447, -4.467917056767334749, 5.799520541027148646 ) ) ;
#4047 = CARTESIAN_POINT ( 'NONE',  ( 6.176542424588119751, -0.9554180641285445752, 5.130639327542137806 ) ) ;
#4048 = CARTESIAN_POINT ( 'NONE',  ( 0.000000000000000000, 0.000000000000000000, 36.00000000000000711 ) ) ;
#4049 = CARTESIAN_POINT ( 'NONE',  ( -5.409007216690642217, -2.598315788643811963, 10.88557478428061032 ) ) ;
#4050 = ORIENTED_EDGE ( 'NONE', *, *, #14901, .T. ) ;
#4051 = CARTESIAN_POINT ( 'NONE',  ( 2.066987300000000083, 186.8999999989075036, 6.143825827087054492 ) ) ;
#4052 = EDGE_LOOP ( 'NONE', ( #13500, #14141, #9232, #10092 ) ) ;
#4053 = DIRECTION ( 'NONE',  ( -0.3090169943749446202, -0.9510565162951544194, 0.000000000000000000 ) ) ;
#4054 =( REPRESENTATION_RELATIONSHIP ('NONE','NONE', #11191, #9569 ) REPRESENTATION_RELATIONSHIP_WITH_TRANSFORMATION ( #2721 )SHAPE_REPRESENTATION_RELATIONSHIP( ) );
#4055 = EDGE_CURVE ( 'NONE', #12288, #4510, #9356, .T. ) ;
#4056 = EDGE_LOOP ( 'NONE', ( #15006, #4955 ) ) ;
#4057 = CARTESIAN_POINT ( 'NONE',  ( -3.061616997868386099E-16, 189.0000000000000000, -7.000000000000000000 ) ) ;
#4058 = CARTESIAN_POINT ( 'NONE',  ( 2.030576276931546336E-13, -6.250000000000000888, 24.49999999999999289 ) ) ;
#4059 = ORIENTED_EDGE ( 'NONE', *, *, #6920, .T. ) ;
#4060 = CARTESIAN_POINT ( 'NONE',  ( 2.066987299999999639, 2.531329380823229670E-16, -1.549999998907525489 ) ) ;
#4061 = CARTESIAN_POINT ( 'NONE',  ( 1.000079958708139261, 5.916066267613699026, 5.131527388820331659 ) ) ;
#4062 = CARTESIAN_POINT ( 'NONE',  ( -1.032108583833363236, 228.1961951329309954, 9.994999926284295455 ) ) ;
#4063 = CARTESIAN_POINT ( 'NONE',  ( 1.461580736456472795, 189.3499999989074922, 5.538419263543527649 ) ) ;
#4064 = CARTESIAN_POINT ( 'NONE',  ( -2.500000000000000444, 1.035533905932737753, -0.7500000000000004441 ) ) ;
#4065 = CARTESIAN_POINT ( 'NONE',  ( 9.750000000000003553, 184.0000000000000000, -1.499999999999897415 ) ) ;
#4066 = CARTESIAN_POINT ( 'NONE',  ( -2.817313151351291012, -5.579000502529380512, 24.49999999999999289 ) ) ;
#4067 = CONTEXT_DEPENDENT_SHAPE_REPRESENTATION ( #12391, #8323 ) ;
#4068 = CARTESIAN_POINT ( 'NONE',  ( 2.500000000000000444, 187.2000000000000171, 7.000000000000000000 ) ) ;
#4069 = CARTESIAN_POINT ( 'NONE',  ( -2.066987299999999639, 0.000000000000000000, -0.9499999989075252893 ) ) ;
#4070 = AXIS2_PLACEMENT_3D ( 'NONE', #15575, #6754, #4357 ) ;
#4071 = CARTESIAN_POINT ( 'NONE',  ( 5.131373506000599605, 7.062729720844090231, 5.000000000000004441 ) ) ;
#4072 = CARTESIAN_POINT ( 'NONE',  ( 1.353717517954364224E-13, -6.000000000000000888, 18.99999999999998934 ) ) ;
#4073 = EDGE_LOOP ( 'NONE', ( #802, #3822 ) ) ;
#4074 = EDGE_LOOP ( 'NONE', ( #13616, #6834, #4532, #2669 ) ) ;
#4075 = ORIENTED_EDGE ( 'NONE', *, *, #2877, .T. ) ;
#4076 = DIRECTION ( 'NONE',  ( -1.000000000000000000, 3.326610055774637112E-18, 1.062480551894331163E-17 ) ) ;
#4077 = CARTESIAN_POINT ( 'NONE',  ( 1.955037903476808836, 189.0000000000000000, 8.565347030709547838 ) ) ;
#4078 = EDGE_LOOP ( 'NONE', ( #1488, #2095, #14503, #3988 ) ) ;
#4079 = CARTESIAN_POINT ( 'NONE',  ( 0.8730628416137207193, 6.188929913094963986, 4.495049298931171222 ) ) ;
#4080 = EDGE_CURVE ( 'NONE', #3329, #14887, #1826, .T. ) ;
#4081 = CARTESIAN_POINT ( 'NONE',  ( 1.000049560716574026, -5.916071405810141570, 30.86967799011530644 ) ) ;
#4082 = CARTESIAN_POINT ( 'NONE',  ( -5.375605342016534394, 2.665598297262232741, 5.503120489023787698 ) ) ;
#4083 = CARTESIAN_POINT ( 'NONE',  ( 0.8499999999999896527, -0.3999999999999941380, -2.619018321873356037 ) ) ;
#4084 = CARTESIAN_POINT ( 'NONE',  ( 1.767766952966368654, 186.1999999978150697, 8.767766952966368876 ) ) ;
#4085 = CARTESIAN_POINT ( 'NONE',  ( -1.767766952966369098, 1.767766952966369098, 1.606999999978150351 ) ) ;
#4086 = CARTESIAN_POINT ( 'NONE',  ( -4.070051655338214225, 4.744673454622383879, 18.87367328635991726 ) ) ;
#4087 = CARTESIAN_POINT ( 'NONE',  ( 0.000000000000000000, 24.00000000000000000, 0.000000000000000000 ) ) ;
#4088 = ADVANCED_FACE ( 'NONE', ( #5171 ), #13666, .T. ) ;
#4089 = B_SPLINE_CURVE_WITH_KNOTS ( 'NONE', 3,
 ( #2693, #8751, #1411, #6369, #7545, #10020, #14867, #12551, #4201, #11127, #13583, #2932, #5249, #14791, #7471, #6524, #10095, #6285 ),
 .UNSPECIFIED., .F., .F.,
 ( 4, 2, 2, 2, 2, 2, 2, 2, 4 ),
 ( 0.000000000000000000, 0.0003914357524127506840, 0.0007828715048255013680, 0.001174307257238252052, 0.001565743009651002736, 0.001957178762063753637, 0.002348614514476504104, 0.002740050266889254571, 0.003131486019302005472 ),
 .UNSPECIFIED. ) ;
#4090 = CARTESIAN_POINT ( 'NONE',  ( -1.035533905932739529, 186.1199999975965511, 9.500000000000003553 ) ) ;
#4091 = CARTESIAN_POINT ( 'NONE',  ( 0.9648499430152943646, 228.2043505555869274, 10.01897217821435859 ) ) ;
#4092 = CARTESIAN_POINT ( 'NONE',  ( -2.257095642740105212, 226.6533546677793538, 5.453940291146690988 ) ) ;
#4093 =( BOUNDED_CURVE ( )  B_SPLINE_CURVE ( 2, ( #627, #11300, #5500, #13680, #10343, #12646, #12796, #15121, #11451 ),
 .UNSPECIFIED., .F., .F. ) 
 B_SPLINE_CURVE_WITH_KNOTS ( ( 3, 2, 2, 2, 3 ),
 ( 0.2857142857142856984, 0.3035714285714285476, 0.3214285714285714524, 0.3392857142857143016, 0.3571428571428571508 ),
 .UNSPECIFIED. ) 
 CURVE ( )  GEOMETRIC_REPRESENTATION_ITEM ( )  RATIONAL_B_SPLINE_CURVE ( ( 1.000000000000000000, 0.9238795325112867385, 1.000000000000000000, 0.9238795325112867385, 1.000000000000000000, 0.9238795325112867385, 1.000000000000000000, 0.9238795325112867385, 1.000000000000000000 ) ) 
 REPRESENTATION_ITEM ( '' )  );
#4094 = EDGE_LOOP ( 'NONE', ( #12733, #10032 ) ) ;
#4095 = CARTESIAN_POINT ( 'NONE',  ( 2.500000000000000444, -1.035533905932737309, 0.5500000021849498211 ) ) ;
#4096 = EDGE_LOOP ( 'NONE', ( #2726, #14804, #12967, #2473 ) ) ;
#4097 = CARTESIAN_POINT ( 'NONE',  ( -5.903843691985208864, 2.055287728870709874, 16.99995093123465750 ) ) ;
#4098 = CARTESIAN_POINT ( 'NONE',  ( -5.558508435838136919, 2.857531096719036601, 24.36936067245786930 ) ) ;
#4099 = CARTESIAN_POINT ( 'NONE',  ( -0.9740856415300837012, 6.173834621338593287, 4.738526530555331462 ) ) ;
#4100 = CARTESIAN_POINT ( 'NONE',  ( -2.066760391300492827E-16, 189.4499999989075150, 4.933012699999999029 ) ) ;
#4101 = EDGE_CURVE ( 'NONE', #11546, #3364, #6527, .T. ) ;
#4102 = CARTESIAN_POINT ( 'NONE',  ( 2.135537325812093989, 227.9676068176768524, 9.322809720636362485 ) ) ;
#4103 = ADVANCED_FACE ( 'NONE', ( #5335 ), #9374, .F. ) ;
#4104 = CARTESIAN_POINT ( 'NONE',  ( 4.267936573529151012, -4.217499624512297984, 24.23770962164067200 ) ) ;
#4105 = CARTESIAN_POINT ( 'NONE',  ( 1.461580736456473018, -1.461580736456472573, -1.449999998907525178 ) ) ;
#4106 = CARTESIAN_POINT ( 'NONE',  ( 2.668367453516629517, 5.373994336898132218, 5.000000000000004441 ) ) ;
#4107 =( NAMED_UNIT ( * ) PLANE_ANGLE_UNIT ( ) SI_UNIT ( $, .RADIAN. ) );
#4108 = CARTESIAN_POINT ( 'NONE',  ( 5.935543223013846514, 0.8771126767607477781, 5.000000000000004441 ) ) ;
#4109 = CARTESIAN_POINT ( 'NONE',  ( -1.767766952966369320, 185.9000000000000057, 5.232233047033630235 ) ) ;
#4110 = CARTESIAN_POINT ( 'NONE',  ( 0.9965032137571403492, 227.6963699622695287, 5.362489989878645780 ) ) ;
#4111 = DIRECTION ( 'NONE',  ( -6.123233995736766036E-17, 1.000000000000000000, 0.000000000000000000 ) ) ;
#4112 = CARTESIAN_POINT ( 'NONE',  ( 1.767766952966369320, -1.767766952966368654, -2.699999997815051067 ) ) ;
#4113 = CARTESIAN_POINT ( 'NONE',  ( 1.461580736456472573, 1.461580736456472795, 0.9500000010924747329 ) ) ;
#4114 = VECTOR ( 'NONE', #11652, 1000.000000000000114 ) ;
#4115 = CARTESIAN_POINT ( 'NONE',  ( 2.066987300000000083, 188.2499999989075263, 7.000000000000000000 ) ) ;
#4116 = CARTESIAN_POINT ( 'NONE',  ( -3.311384659207262882, 5.004923837169336309, 18.97358595436693207 ) ) ;
#4118 = ORIENTED_EDGE ( 'NONE', *, *, #9073, .T. ) ;
#4117 = CARTESIAN_POINT ( 'NONE',  ( -1.461580736456473018, 188.7499999989075263, 5.538419263543527649 ) ) ;
#4119 = CARTESIAN_POINT ( 'NONE',  ( -3.567624405365327878, -5.133384272590721054, 17.00004921015705861 ) ) ;
#4120 = CARTESIAN_POINT ( 'NONE',  ( 1.035533905932738197, 186.9499999978150413, 9.500000000000000000 ) ) ;
#4121 = CARTESIAN_POINT ( 'NONE',  ( 0.4244143561419055910, 0.4000000000000062395, -2.581346380257607986 ) ) ;
#4122 = FILL_AREA_STYLE_COLOUR ( '', #738 ) ;
#4123 = AXIS2_PLACEMENT_3D ( 'NONE', #12259, #8464, #169 ) ;
#4124 = CARTESIAN_POINT ( 'NONE',  ( 3.013685100799304184, 189.2999267616114878, 7.018152099054431048 ) ) ;
#4125 = DIRECTION ( 'NONE',  ( 0.000000000000000000, 1.000000000000000000, 0.000000000000000000 ) ) ;
#4126 = CARTESIAN_POINT ( 'NONE',  ( 5.317509234264001350, -2.779225709350912954, 11.49999999999998224 ) ) ;
#4127 = CARTESIAN_POINT ( 'NONE',  ( 7.490007020835706797, -2.433650805992179755, 11.49999999999998224 ) ) ;
#4128 = CARTESIAN_POINT ( 'NONE',  ( 9.750000000000003553, 19.99999999999999645, -1.499999999999897415 ) ) ;
#4129 = CARTESIAN_POINT ( 'NONE',  ( -5.935543223013839409, -0.8771126767608162789, 11.36763921416086554 ) ) ;
#4130 = EDGE_LOOP ( 'NONE', ( #11932, #1000, #3119, #8503 ) ) ;
#4131 = CARTESIAN_POINT ( 'NONE',  ( -2.066987300000001415, 188.0999999989074922, 7.856174172912944620 ) ) ;
#4132 = ORIENTED_EDGE ( 'NONE', *, *, #7757, .F. ) ;
#4133 = CARTESIAN_POINT ( 'NONE',  ( -5.935543223013831415, 0.8771126767608680153, 24.49999999999999289 ) ) ;
#4134 = ORIENTED_EDGE ( 'NONE', *, *, #4680, .T. ) ;
#4135 = AXIS2_PLACEMENT_3D ( 'NONE', #14602, #13398, #12282 ) ;
#4136 = LINE ( 'NONE', #2869, #13682 ) ;
#4137 = ORIENTED_EDGE ( 'NONE', *, *, #14948, .F. ) ;
#4138 = CARTESIAN_POINT ( 'NONE',  ( -3.312341048453360415, -5.004306261885527185, 5.973980201222397923 ) ) ;
#4139 = CARTESIAN_POINT ( 'NONE',  ( -2.500000000000000000, 0.000000000000000000, -1.500000000000000000 ) ) ;
#4140 = CARTESIAN_POINT ( 'NONE',  ( -0.5043776560896817696, 6.230795654995842980, 25.37337476296002947 ) ) ;
#4141 = CARTESIAN_POINT ( 'NONE',  ( 0.4831378333609244180, 2.500000000000000000, -2.523327958195909826 ) ) ;
#4142 = DIRECTION ( 'NONE',  ( 0.000000000000000000, 0.000000000000000000, -1.000000000000000000 ) ) ;
#4143 = CARTESIAN_POINT ( 'NONE',  ( -4.196288036172528990, 4.288789315524756951, 17.49687951097622474 ) ) ;
#4144 = ADVANCED_FACE ( 'NONE', ( #7069 ), #12782, .F. ) ;
#4145 = ITEM_DEFINED_TRANSFORMATION ( 'NONE', 'NONE', #9341,  #14201 ) ;
#4146 = DIRECTION ( 'NONE',  ( 1.000000000000000000, 0.000000000000000000, 0.000000000000000000 ) ) ;
#4147 = CARTESIAN_POINT ( 'NONE',  ( 2.066987299999999639, 0.8561741729129456191, 1.100000001092475088 ) ) ;
#4148 = CARTESIAN_POINT ( 'NONE',  ( 3.421280866381083641, 4.930711975950953452, 12.50004932073310471 ) ) ;
#4149 = ADVANCED_FACE ( 'NONE', ( #6840 ), #12944, .F. ) ;
#4150 = VERTEX_POINT ( 'NONE', #10412 ) ;
#4151 = ORIENTED_EDGE ( 'NONE', *, *, #10955, .F. ) ;
#4152 = ADVANCED_FACE ( 'NONE', ( #10563 ), #14974, .T. ) ;
#4153 = VERTEX_POINT ( 'NONE', #655 ) ;
#4154 = CARTESIAN_POINT ( 'NONE',  ( 4.153440676704430956, -4.671190581744464332, 12.29954462468842813 ) ) ;
#4155 = DIRECTION ( 'NONE',  ( -0.000000000000000000, 1.000000000000000000, -0.000000000000000000 ) ) ;
#4156 = B_SPLINE_CURVE_WITH_KNOTS ( 'NONE', 3,
 ( #4350, #9285, #10319, #5476, #8169, #14121, #764, #1795, #3227, #9209, #11738, #8008, #12930, #12849, #5628, #10475, #9135, #12769 ),
 .UNSPECIFIED., .F., .F.,
 ( 4, 2, 2, 2, 2, 2, 2, 2, 4 ),
 ( 0.003131918686235975191, 0.003523310662250265460, 0.003914702638264555730, 0.004306094614278846433, 0.004697486590293136269, 0.005088878566307426972, 0.005480270542321717675, 0.005871662518336007511, 0.006263054494350298214 ),
 .UNSPECIFIED. ) ;
#4157 = VERTEX_POINT ( 'NONE', #14250 ) ;
#4158 = DIRECTION ( 'NONE',  ( 0.000000000000000000, 0.000000000000000000, 1.000000000000000000 ) ) ;
#4159 = AXIS2_PLACEMENT_3D ( 'NONE', #10804, #14463, #7235 ) ;
#4160 = CARTESIAN_POINT ( 'NONE',  ( 0.7993401192313105419, -6.199366368793645776, 18.61483246936574432 ) ) ;
#4161 = EDGE_CURVE ( 'NONE', #6307, #2787, #2430, .T. ) ;
#4162 = CARTESIAN_POINT ( 'NONE',  ( -5.665308849928848645, 1.980336949702434790, 5.999920023562623328 ) ) ;
#4163 = CARTESIAN_POINT ( 'NONE',  ( -1.767766952966369765, 187.5999999978150754, 8.767766952966368876 ) ) ;
#4164 = CARTESIAN_POINT ( 'NONE',  ( -6.369687763352338550E-16, 186.8999999978150584, 9.500000000000001776 ) ) ;
#4165 = CARTESIAN_POINT ( 'NONE',  ( -4.322356511625788045, 7.650514973136498753, 31.00000000000000000 ) ) ;
#4166 = CARTESIAN_POINT ( 'NONE',  ( 0.000000000000000000, 184.0000000000000000, 0.000000000000000000 ) ) ;
#4167 = CARTESIAN_POINT ( 'NONE',  ( -2.500000000000000444, 186.7199999975965454, 5.964466094067261359 ) ) ;
#4168 = CARTESIAN_POINT ( 'NONE',  ( 1.978507955918972439, 228.0159604248740663, 9.465015589616863068 ) ) ;
#4169 = CARTESIAN_POINT ( 'NONE',  ( -2.548643141829932901, 227.7997363639018147, 8.829041127271985090 ) ) ;
#4170 = ORIENTED_EDGE ( 'NONE', *, *, #12599, .T. ) ;
#4171 = CARTESIAN_POINT ( 'NONE',  ( 4.286401442266591921, -4.198423832313132209, 5.000000000000004441 ) ) ;
#4172 =( BOUNDED_CURVE ( )  B_SPLINE_CURVE ( 2, ( #9676, #3451, #6970, #8319, #7128, #7207, #13158, #11803, #10621 ),
 .UNSPECIFIED., .F., .F. ) 
 B_SPLINE_CURVE_WITH_KNOTS ( ( 3, 2, 2, 2, 3 ),
 ( 0.5000000000000000000, 0.5178571428571429047, 0.5357142857142856984, 0.5535714285714286031, 0.5714285714285713969 ),
 .UNSPECIFIED. ) 
 CURVE ( )  GEOMETRIC_REPRESENTATION_ITEM ( )  RATIONAL_B_SPLINE_CURVE ( ( 1.000000000000000000, 0.9238795325112867385, 1.000000000000000000, 0.9238795325112867385, 1.000000000000000000, 0.9238795325112867385, 1.000000000000000000, 0.9238795325112867385, 1.000000000000000000 ) ) 
 REPRESENTATION_ITEM ( '' )  );
#4173 = ORIENTED_EDGE ( 'NONE', *, *, #11196, .T. ) ;
#4174 = DIRECTION ( 'NONE',  ( -1.000000000000000000, 3.326610055774637112E-18, 1.062480551894331163E-17 ) ) ;
#4175 = CIRCLE ( 'NONE', #14322, 1.499999999999999556 ) ;
#4176 = CARTESIAN_POINT ( 'NONE',  ( 1.767766952966369098, 189.5999999978150470, 5.232233047033630235 ) ) ;
#4177 = CARTESIAN_POINT ( 'NONE',  ( 0.6139731865240710684, -6.220476368274045598, 10.69975545601931799 ) ) ;
#4178 = CYLINDRICAL_SURFACE ( 'NONE', #13943, 1.000000000000000888 ) ;
#4179 = CARTESIAN_POINT ( 'NONE',  ( 1.485919012929320271, 228.1288645930629286, 9.797042361818872891 ) ) ;
#4180 = CARTESIAN_POINT ( 'NONE',  ( 3.922288969639700529, -4.542045818322596240, 23.62621569129737154 ) ) ;
#4181 = EDGE_CURVE ( 'NONE', #12139, #2516, #8147, .T. ) ;
#4182 = CARTESIAN_POINT ( 'NONE',  ( 6.176542424588121527, -0.9554180641285238140, 31.00000000000000000 ) ) ;
#4183 = CARTESIAN_POINT ( 'NONE',  ( 0.8561741729129463963, -2.066987299999999195, -1.499999998907525445 ) ) ;
#4184 = CARTESIAN_POINT ( 'NONE',  ( -3.420311045507770764, -4.931422832349343643, 32.00007961174477344 ) ) ;
#4185 = CARTESIAN_POINT ( 'NONE',  ( -2.997451966578355886, -5.485105005466039074, 30.38482219624157565 ) ) ;
#4186 = CARTESIAN_POINT ( 'NONE',  ( 2.500000000000000444, 187.2000000000000171, 7.000000000000000000 ) ) ;
#4187 = AXIS2_PLACEMENT_3D ( 'NONE', #5193, #6159, #255 ) ;
#4188 = CARTESIAN_POINT ( 'NONE',  ( -1.724657202313207849, 227.9349080091615178, 6.051401474621576071 ) ) ;
#4189 = PRODUCT_DEFINITION_CONTEXT ( 'detailed design', #4761, 'design' ) ;
#4190 = LINE ( 'NONE', #11737, #2459 ) ;
#4191 = EDGE_CURVE ( 'NONE', #11875, #11314, #12308, .T. ) ;
#4192 = CARTESIAN_POINT ( 'NONE',  ( -4.152999119457986055, -4.671604476854346544, 10.69973484982324052 ) ) ;
#4193 = CARTESIAN_POINT ( 'NONE',  ( -0.8561741729129458411, -2.066987299999999195, -0.1999999989075254836 ) ) ;
#4194 = CARTESIAN_POINT ( 'NONE',  ( -1.767766952966369542, 185.2999999999999829, 8.767766952966368876 ) ) ;
#4195 = CARTESIAN_POINT ( 'NONE',  ( -5.329907877631296031, -2.755840666746375511, 18.26194324003145653 ) ) ;
#4196 = EDGE_CURVE ( 'NONE', #14255, #11999, #8150, .T. ) ;
#4198 = EDGE_LOOP ( 'NONE', ( #14714, #12249 ) ) ;
#4197 = CARTESIAN_POINT ( 'NONE',  ( -5.895349312889930360E-16, 187.4499999989075150, 9.066987300000000971 ) ) ;
#4199 = CARTESIAN_POINT ( 'NONE',  ( -4.344502777243583580, -4.493369211529213203, 17.49610786875029689 ) ) ;
#4200 = AXIS2_PLACEMENT_3D ( 'NONE', #7400, #9870, #6218 ) ;
#4201 = CARTESIAN_POINT ( 'NONE',  ( 5.903596343266319657, -2.055998103990523518, 12.49995078984291830 ) ) ;
#4202 = B_SPLINE_CURVE_WITH_KNOTS ( 'NONE', 3,
 ( #12109, #2490, #14329, #10840, #7348, #3521, #24, #4886, #4968, #3436, #12190, #7194, #11950, #1289, #6163, #9819, #1132, #10766 ),
 .UNSPECIFIED., .F., .F.,
 ( 4, 2, 2, 2, 2, 2, 2, 2, 4 ),
 ( 0.003131486019301987257, 0.003522824630466693530, 0.003914163241631398935, 0.004305501852796105207, 0.004696840463960811479, 0.005088179075125518619, 0.005479517686290224891, 0.005870856297454931164, 0.006262194908619638303 ),
 .UNSPECIFIED. ) ;
#4203 = CARTESIAN_POINT ( 'NONE',  ( 0.01327486276323468564, 190.0875178197512696, 4.201689379953597481 ) ) ;
#4204 =( LENGTH_UNIT ( ) NAMED_UNIT ( * ) SI_UNIT ( .MILLI., .METRE. ) );
#4205 = CARTESIAN_POINT ( 'NONE',  ( 2.348212394088349253, 189.9869324597729587, 5.353485886314879316 ) ) ;
#4206 = CARTESIAN_POINT ( 'NONE',  ( 7.180990026460741582, -3.384707322287397790, 5.000000000000004441 ) ) ;
#4207 = CARTESIAN_POINT ( 'NONE',  ( -2.817313151351249711, 5.579000502529400940, 11.49999999999998224 ) ) ;
#4208 = CARTESIAN_POINT ( 'NONE',  ( 0.07962197837297851910, 190.0874091994478761, 4.202769589527710181 ) ) ;
#4209 = CARTESIAN_POINT ( 'NONE',  ( 5.858736126997154514, -2.179962889277010873, 5.973595717233013858 ) ) ;
#4210 = CARTESIAN_POINT ( 'NONE',  ( -2.066987299999999639, 0.000000000000000000, 2.250000001092474999 ) ) ;
#4211 = CARTESIAN_POINT ( 'NONE',  ( -5.935543223013836744, -0.8771126767608161678, 11.49999999999998224 ) ) ;
#4212 = EDGE_LOOP ( 'NONE', ( #12683, #13543 ) ) ;
#4213 = CARTESIAN_POINT ( 'NONE',  ( 0.8561741729129461742, 184.8999999989075320, 9.066987300000000971 ) ) ;
#4214 = VERTEX_POINT ( 'NONE', #11863 ) ;
#4215 = CARTESIAN_POINT ( 'NONE',  ( -5.915641100987789613, -1.003868594704996342, 23.99571079637979665 ) ) ;
#4216 = ORIENTED_EDGE ( 'NONE', *, *, #13485, .F. ) ;
#4217 = LINE ( 'NONE', #13914, #10145 ) ;
#4218 = DIRECTION ( 'NONE',  ( 0.000000000000000000, 0.000000000000000000, 1.000000000000000000 ) ) ;
#4219 = CARTESIAN_POINT ( 'NONE',  ( -0.8561741729129455081, 2.066987299999999639, -2.899999998907526244 ) ) ;
#4220 = CARTESIAN_POINT ( 'NONE',  ( -0.1323933160974262724, 6.000000000000003553, 18.99999999999998934 ) ) ;
#4221 = CARTESIAN_POINT ( 'NONE',  ( -4.416678568553632722, -4.422441866694328816, 5.262369734438752999 ) ) ;
#4222 = CARTESIAN_POINT ( 'NONE',  ( 1.767766952966369320, -1.767766952966368654, -2.000000000000000444 ) ) ;
#4223 = CARTESIAN_POINT ( 'NONE',  ( -6.081464507797627483, -1.446657058464217327, 5.873800552473966263 ) ) ;
#4224 = DIRECTION ( 'NONE',  ( 0.000000000000000000, 1.000000000000000000, 0.000000000000000000 ) ) ;
#4225 = DIRECTION ( 'NONE',  ( -0.3090169943749446202, -0.9510565162951544194, 0.000000000000000000 ) ) ;
#4226 = CARTESIAN_POINT ( 'NONE',  ( 1.461580736456472573, 1.461580736456472795, -1.249999998907525223 ) ) ;
#4227 = CARTESIAN_POINT ( 'NONE',  ( 2.848235266350948702, 5.281699484015686785, 12.11397738943082736 ) ) ;
#4228 = EDGE_CURVE ( 'NONE', #6465, #8099, #9659, .T. ) ;
#4229 = ORIENTED_EDGE ( 'NONE', *, *, #3504, .T. ) ;
#4230 = EDGE_LOOP ( 'NONE', ( #509, #7952, #10338, #2455 ) ) ;
#4231 = AXIS2_PLACEMENT_3D ( 'NONE', #12227, #6201, #11038 ) ;
#4232 = VERTEX_POINT ( 'NONE', #14414 ) ;
#4233 = CARTESIAN_POINT ( 'NONE',  ( 4.344265632482078310, -4.493596842504967270, 18.50425949503009448 ) ) ;
#4234 = CARTESIAN_POINT ( 'NONE',  ( 0.000000000000000000, 2.000000000000000000, -13.50000000000000000 ) ) ;
#4235 = ORIENTED_EDGE ( 'NONE', *, *, #5424, .F. ) ;
#4236 = CARTESIAN_POINT ( 'NONE',  ( 5.931828553037993501, -0.9033193133617988257, 18.26194324003146008 ) ) ;
#4237 = EDGE_CURVE ( 'NONE', #7182, #15136, #1053, .T. ) ;
#4238 = CARTESIAN_POINT ( 'NONE',  ( 2.500000000000000444, 1.035533905932737975, -0.1499999978150504398 ) ) ;
#4239 = CARTESIAN_POINT ( 'NONE',  ( -5.903057025253926504, 1.078199533779401253, 5.615617326986045654 ) ) ;
#4240 = CARTESIAN_POINT ( 'NONE',  ( 5.649200442566188585, -2.675373855294086667, 30.38439807107076973 ) ) ;
#4241 = CARTESIAN_POINT ( 'NONE',  ( -2.500000000000000888, 189.0999999978150470, 7.000000000000000000 ) ) ;
#4242 = CARTESIAN_POINT ( 'NONE',  ( -5.131373506000823426, 7.062729720843950787, 17.99999999999998934 ) ) ;
#4243 = CARTESIAN_POINT ( 'NONE',  ( 5.843318061569063637, 1.367618216965549749, 18.87303779027049444 ) ) ;
#4244 = DIRECTION ( 'NONE',  ( 1.000000000000000000, 0.000000000000000000, 0.000000000000000000 ) ) ;
#4245 = ADVANCED_FACE ( 'NONE', ( #9743 ), #3596, .T. ) ;
#4246 = CARTESIAN_POINT ( 'NONE',  ( -5.620879908643960476, -2.102487719021914003, 4.026221760567070262 ) ) ;
#4247 = CARTESIAN_POINT ( 'NONE',  ( -1.826974499845722466, 228.5193582813216153, 7.739327195479140720 ) ) ;
#4248 = CARTESIAN_POINT ( 'NONE',  ( -2.998822209637060254, 227.3208645008386668, 7.419865387590665939 ) ) ;
#4249 = ORIENTED_EDGE ( 'NONE', *, *, #6301, .T. ) ;
#4250 = CARTESIAN_POINT ( 'NONE',  ( -0.4013174258278009998, -2.483589256803624412, -2.498872199792083304 ) ) ;
#4251 = B_SPLINE_CURVE_WITH_KNOTS ( 'NONE', 3,
 ( #15112, #6922, #10567, #4523, #5570, #781, #1890, #8110, #6765, #13987, #7873, #696, #10416, #14061, #8026, #1968, #6845, #9080, #5643 ),
 .UNSPECIFIED., .F., .F.,
 ( 4, 3, 3, 3, 3, 3, 4 ),
 ( 0.0003917759849713744504, 0.0004043855146501730080, 0.0004375639695040863583, 0.0004708920258237459097, 0.0005045670765489163306, 0.0005386560839275773317, 0.0005403960448094325937 ),
 .UNSPECIFIED. ) ;
#4252 = ORIENTED_EDGE ( 'NONE', *, *, #3989, .T. ) ;
#4253 = CARTESIAN_POINT ( 'NONE',  ( -0.7993401192311344605, 6.199366368793667981, 12.11483246936570524 ) ) ;
#4254 = CIRCLE ( 'NONE', #9097, 5.000000000000000000 ) ;
#4255 = EDGE_CURVE ( 'NONE', #4510, #12288, #14712, .T. ) ;
#4256 = CARTESIAN_POINT ( 'NONE',  ( 1.767766952966368432, 189.3999999978150584, 8.767766952966368876 ) ) ;
#4257 = CARTESIAN_POINT ( 'NONE',  ( 2.066987300000000971, 184.2999999989074809, 6.143825827087054492 ) ) ;
#4258 = FACE_BOUND ( 'NONE', #12870, .T. ) ;
#4259 = CYLINDRICAL_SURFACE ( 'NONE', #4888, 12.50000000000000355 ) ;
#4260 = CARTESIAN_POINT ( 'NONE',  ( 3.883716939929077849, 4.898343590941176551, 5.973595717233015634 ) ) ;
#4261 = CARTESIAN_POINT ( 'NONE',  ( 2.817313151351065859, -5.579000502529494199, 17.99999999999998934 ) ) ;
#4262 = CARTESIAN_POINT ( 'NONE',  ( -1.767766952966369098, 1.767766952966369098, -0.7999999999999999334 ) ) ;
#4263 = FACE_OUTER_BOUND ( 'NONE', #5596, .T. ) ;
#4264 = EDGE_CURVE ( 'NONE', #8559, #13449, #9369, .T. ) ;
#4265 = PRODUCT_DEFINITION_FORMATION_WITH_SPECIFIED_SOURCE ( 'ANY', '', #6017, .NOT_KNOWN. ) ;
#4266 = CARTESIAN_POINT ( 'NONE',  ( 0.06610679800811947171, 0.4000000000000045186, -2.546908780914493242 ) ) ;
#4267 = CARTESIAN_POINT ( 'NONE',  ( 1.035533905932737753, 188.1499999999999773, 4.500000000000000888 ) ) ;
#4268 = CARTESIAN_POINT ( 'NONE',  ( 1.454231928715901123, 227.8150477629479269, 5.705238247175231869 ) ) ;
#4269 = FACE_BOUND ( 'NONE', #4073, .T. ) ;
#4270 = CARTESIAN_POINT ( 'NONE',  ( -7.180990026460747799, -3.384707322287517695, 5.000000000000004441 ) ) ;
#4271 = CARTESIAN_POINT ( 'NONE',  ( 2.066987299999999639, 0.8561741729129456191, -1.499999998907525445 ) ) ;
#4272 = CARTESIAN_POINT ( 'NONE',  ( 1.767766952966368432, 186.2999999999999829, 8.767766952966368876 ) ) ;
#4273 = PLANE ( 'NONE',  #13917 ) ;
#4274 = VECTOR ( 'NONE', #4529, 1000.000000000000114 ) ;
#4276 = ORIENTED_EDGE ( 'NONE', *, *, #12836, .F. ) ;
#4275 = CARTESIAN_POINT ( 'NONE',  ( 1.035533905932737531, 2.500000000000000444, -1.649999997815050579 ) ) ;
#4277 = CARTESIAN_POINT ( 'NONE',  ( -3.827021247335478803E-16, 2.500000000000000000, -2.500000000000000000 ) ) ;
#4278 = VECTOR ( 'NONE', #462, 1000.000000000000000 ) ;
#4279 = CARTESIAN_POINT ( 'NONE',  ( -0.5030929395820217254, -6.230885867001147105, 4.126003191165496631 ) ) ;
#4280 = ADVANCED_FACE ( 'NONE', ( #1130 ), #10838, .F. ) ;
#4281 = CARTESIAN_POINT ( 'NONE',  ( -5.931817299736832361, 0.9033986943603389275, 24.23770962164067200 ) ) ;
#4282 = CARTESIAN_POINT ( 'NONE',  ( 1.857821011765909747, 189.1149986214457783, 9.541363111238132078 ) ) ;
#4283 = CARTESIAN_POINT ( 'NONE',  ( 1.035533905932737753, 188.0499999978150356, 4.500000000000001776 ) ) ;
#4284 = CARTESIAN_POINT ( 'NONE',  ( -0.0007128680628333008105, 227.6089742637946642, 5.110086227958842819 ) ) ;
#4285 = CARTESIAN_POINT ( 'NONE',  ( 1.211961328308884367, 228.7773363860045492, 8.484382675910040916 ) ) ;
#4287 = CARTESIAN_POINT ( 'NONE',  ( 5.649200442566265856, -2.675373855293923686, 23.88439807107078039 ) ) ;
#4286 = CIRCLE ( 'NONE', #14709, 6.000000000000000888 ) ;
#4288 = CARTESIAN_POINT ( 'NONE',  ( -5.570722351696298702, 2.834100162821898916, 4.738097869159890507 ) ) ;
#4289 = CARTESIAN_POINT ( 'NONE',  ( -3.922672396097018233, -4.541739265057732844, 30.12635295315576656 ) ) ;
#4290 = ORIENTED_EDGE ( 'NONE', *, *, #2340, .T. ) ;
#4291 = CARTESIAN_POINT ( 'NONE',  ( -2.066987300000001415, 186.2999999989075093, 7.856174172912944620 ) ) ;
#4292 = CARTESIAN_POINT ( 'NONE',  ( 1.767766952966368654, 184.7000000000000171, 8.767766952966368876 ) ) ;
#4293 = ORIENTED_EDGE ( 'NONE', *, *, #8957, .T. ) ;
#4294 = DIRECTION ( 'NONE',  ( 0.8090169943749421222, 0.5877852522924802425, 0.000000000000000000 ) ) ;
#4295 = SURFACE_SIDE_STYLE ('',( #323 ) ) ;
#4296 = VECTOR ( 'NONE', #8334, 1000.000000000000000 ) ;
#4297 = AXIS2_PLACEMENT_3D ( 'NONE', #15276, #3177, #11917 ) ;
#4298 = CARTESIAN_POINT ( 'NONE',  ( 9.750000000000003553, 22.00000000000000000, -1.499999999999897415 ) ) ;
#4299 = CARTESIAN_POINT ( 'NONE',  ( 0.1323602877612205797, 6.000000000000001776, 6.000000000000007105 ) ) ;
#4300 = CARTESIAN_POINT ( 'NONE',  ( 2.066987300000000527, 184.2999999989075093, 6.143825827087054492 ) ) ;
#4301 = EDGE_CURVE ( 'NONE', #11794, #13528, #836, .T. ) ;
#4302 = CARTESIAN_POINT ( 'NONE',  ( 5.665707375537527568, -1.979196487016524175, 23.49992038825522300 ) ) ;
#4303 = CARTESIAN_POINT ( 'NONE',  ( 1.767766952966368654, 1.767766952966369098, -1.800000000000000044 ) ) ;
#4304 = CARTESIAN_POINT ( 'NONE',  ( -6.155867707731109917, -1.081837891425901921, 5.504369696801525436 ) ) ;
#4305 = CARTESIAN_POINT ( 'NONE',  ( -5.999999999999999112, 185.8606548077538321, 9.048340948986950849 ) ) ;
#4306 = CYLINDRICAL_SURFACE ( 'NONE', #6487, 1.000000000000000666 ) ;
#4307 = CARTESIAN_POINT ( 'NONE',  ( 2.930922878467487003, 5.520395124723568081, 31.50389213124968890 ) ) ;
#4308 = CARTESIAN_POINT ( 'NONE',  ( -0.6151877315909831667, 6.220340188096017187, 31.79906673469668732 ) ) ;
#4309 = ORIENTED_EDGE ( 'NONE', *, *, #12116, .T. ) ;
#4310 =( GEOMETRIC_REPRESENTATION_CONTEXT ( 3 ) GLOBAL_UNCERTAINTY_ASSIGNED_CONTEXT ( ( #2502 ) ) GLOBAL_UNIT_ASSIGNED_CONTEXT ( ( #2041, #14210, #4679 ) ) REPRESENTATION_CONTEXT ( 'NONE', 'WORKASPACE' ) );
#4311 = ORIENTED_EDGE ( 'NONE', *, *, #12250, .T. ) ;
#4312 = AXIS2_PLACEMENT_3D ( 'NONE', #9668, #14509, #7041 ) ;
#4313 = ORIENTED_EDGE ( 'NONE', *, *, #9207, .F. ) ;
#4314 = CARTESIAN_POINT ( 'NONE',  ( -5.858813228503623627, -2.179803269293346002, 10.52622717124729412 ) ) ;
#4315 = CARTESIAN_POINT ( 'NONE',  ( 0.000000000000000000, 0.000000000000000000, -5.500000000000000000 ) ) ;
#4316 = ORIENTED_EDGE ( 'NONE', *, *, #2542, .F. ) ;
#4317 = CARTESIAN_POINT ( 'NONE',  ( -2.500000000000000000, -1.035533905932739307, 0.2500000021849494991 ) ) ;
#4318 = CARTESIAN_POINT ( 'NONE',  ( -5.931817299736849236, -0.9033986943602401176, 31.26229037835932090 ) ) ;
#4319 = STYLED_ITEM ( 'NONE', ( #11033 ), #4613 ) ;
#4320 = CARTESIAN_POINT ( 'NONE',  ( -2.817313151351109379, -5.579000502529471994, 5.000000000000004441 ) ) ;
#4321 = CARTESIAN_POINT ( 'NONE',  ( 2.500000000000000444, 189.5499999978150640, 5.964466094067262247 ) ) ;
#4322 = AXIS2_PLACEMENT_3D ( 'NONE', #10172, #10019, #14866 ) ;
#4323 = CARTESIAN_POINT ( 'NONE',  ( 1.035533905932737531, 2.500000000000000444, 2.256999999978151372 ) ) ;
#4324 = CARTESIAN_POINT ( 'NONE',  ( 3.106366801611939010, 5.134708448381321233, 10.62696220972947181 ) ) ;
#4325 = B_SPLINE_CURVE_WITH_KNOTS ( 'NONE', 3,
 ( #1838, #3194, #3042, #725, #10518, #12736, #6638, #12665, #5364, #15293, #9174, #2965, #4154, #3120, #8132, #15061, #1762, #11468 ),
 .UNSPECIFIED., .F., .F.,
 ( 4, 2, 2, 2, 2, 2, 2, 2, 4 ),
 ( 0.003131486019301968175, 0.003522824630466676616, 0.003914163241631385057, 0.004305501852796093064, 0.004696840463960801071, 0.005088179075125509945, 0.005479517686290218820, 0.005870856297454928562, 0.006262194908619637436 ),
 .UNSPECIFIED. ) ;
#4326 = ITEM_DEFINED_TRANSFORMATION ( 'NONE', 'NONE', #9669,  #14201 ) ;
#4327 = CARTESIAN_POINT ( 'NONE',  ( -2.066987299999999639, 0.8561741729129452860, 1.200000001092474733 ) ) ;
#4328 = CARTESIAN_POINT ( 'NONE',  ( 2.500000000000000444, 189.6199999975965795, 5.964466094067262247 ) ) ;
#4329 = CARTESIAN_POINT ( 'NONE',  ( -0.06495987523897406302, 228.9118723585069120, 8.872930237925691799 ) ) ;
#4330 = B_SPLINE_CURVE_WITH_KNOTS ( 'NONE', 3,
 ( #13494, #4997, #9849, #7307, #1167, #2361, #13181, #3557, #9698, #6120, #9357, #14535, #13421, #8510, #8587, #15657, #5954, #11111 ),
 .UNSPECIFIED., .F., .F.,
 ( 4, 2, 2, 2, 2, 2, 2, 2, 4 ),
 ( 0.003131486019301969476, 0.003522824630466678351, 0.003914163241631387659, 0.004305501852796096533, 0.004696840463960805408, 0.005088179075125515149, 0.005479517686290224024, 0.005870856297454932898, 0.006262194908619641773 ),
 .UNSPECIFIED. ) ;
#4331 = CARTESIAN_POINT ( 'NONE',  ( -2.710505431213761085E-17, 228.2551366889530016, 10.16828399152529983 ) ) ;
#4332 = EDGE_LOOP ( 'NONE', ( #10442, #4892, #5062, #9176 ) ) ;
#4333 = CARTESIAN_POINT ( 'NONE',  ( 2.502037656352691375, 0.09969062346262420882, -2.500435595467218164 ) ) ;
#4334 = ORIENTED_EDGE ( 'NONE', *, *, #2149, .T. ) ;
#4335 = CYLINDRICAL_SURFACE ( 'NONE', #8619, 1.000000000000000666 ) ;
#4336 = DIRECTION ( 'NONE',  ( -0.3090169943749446202, -0.9510565162951544194, 0.000000000000000000 ) ) ;
#4337 = CARTESIAN_POINT ( 'NONE',  ( -0.5044069930203394225, 5.979990686694992341, 5.873357432279042278 ) ) ;
#4338 = ORIENTED_EDGE ( 'NONE', *, *, #364, .T. ) ;
#4339 = CARTESIAN_POINT ( 'NONE',  ( 0.000000000000000000, 19.99999999999999645, 0.000000000000000000 ) ) ;
#4340 = CARTESIAN_POINT ( 'NONE',  ( -1.000082492230513820, -6.169467968613740361, 24.63152538105391187 ) ) ;
#4341 = SURFACE_STYLE_FILL_AREA ( #9198 ) ;
#4342 = CARTESIAN_POINT ( 'NONE',  ( -1.767766952966368432, -1.767766952966369320, -0.6000000000000003109 ) ) ;
#4343 = CARTESIAN_POINT ( 'NONE',  ( 3.106366801611989636, 5.134708448381291035, 4.126962209729496678 ) ) ;
#4344 = CARTESIAN_POINT ( 'NONE',  ( -7.180990026460740694, -3.384707322287537679, 31.00000000000000000 ) ) ;
#4345 = CARTESIAN_POINT ( 'NONE',  ( 1.035533905932737975, 186.4499999978150697, 4.500000000000000888 ) ) ;
#4346 = ADVANCED_FACE ( 'NONE', ( #2488 ), #7346, .F. ) ;
#4347 = CARTESIAN_POINT ( 'NONE',  ( -1.923824245924939058, 228.4291822535419954, 7.478893683947804405 ) ) ;
#4348 = PRODUCT_DEFINITION_CONTEXT ( 'detailed design', #8009, 'design' ) ;
#4349 = FACE_BOUND ( 'NONE', #13700, .T. ) ;
#4350 = CARTESIAN_POINT ( 'NONE',  ( -5.317509234263906315, 2.779225709351095475, 17.99999999999998934 ) ) ;
#4351 = EDGE_CURVE ( 'NONE', #8237, #15509, #14960, .T. ) ;
#4352 = CARTESIAN_POINT ( 'NONE',  ( 3.796994071234844259E-16, -2.066987299999999639, -2.549999998907525267 ) ) ;
#4353 = CARTESIAN_POINT ( 'NONE',  ( -2.500000000000000444, 186.0500000000000114, 8.035533905932737753 ) ) ;
#4354 = CARTESIAN_POINT ( 'NONE',  ( 3.253823204785034839, -5.337590213880554657, 25.37305891554299464 ) ) ;
#4356 = ORIENTED_EDGE ( 'NONE', *, *, #3349, .F. ) ;
#4355 = CARTESIAN_POINT ( 'NONE',  ( 2.500000000000000444, 1.035533905932737975, -1.749999997815050445 ) ) ;
#4357 = DIRECTION ( 'NONE',  ( 0.000000000000000000, -0.000000000000000000, 1.000000000000000000 ) ) ;
#4358 = B_SPLINE_CURVE_WITH_KNOTS ( 'NONE', 3,
 ( #13448, #4947, #5979, #8452, #9798, #14648, #1349, #14729, #6224, #3816, #13519, #2626, #7482, #12326, #7874, #2783, #13671, #6459 ),
 .UNSPECIFIED., .F., .F.,
 ( 4, 2, 2, 2, 2, 2, 2, 2, 4 ),
 ( 0.003131918686235980395, 0.003523310662250270665, 0.003914702638264560934, 0.004306094614278851637, 0.004697486590293141473, 0.005088878566307432176, 0.005480270542321721144, 0.005871662518336010980, 0.006263054494350299949 ),
 .UNSPECIFIED. ) ;
#4359 = FACE_OUTER_BOUND ( 'NONE', #2389, .T. ) ;
#4360 = CARTESIAN_POINT ( 'NONE',  ( -0.3990466364818540668, 190.0854366310740318, 4.222250755151196522 ) ) ;
#4361 = CARTESIAN_POINT ( 'NONE',  ( 0.000000000000000000, 0.000000000000000000, 0.000000000000000000 ) ) ;
#4362 = CARTESIAN_POINT ( 'NONE',  ( 0.000000000000000000, 184.0000000000000000, 7.000000000000000000 ) ) ;
#4363 = CARTESIAN_POINT ( 'NONE',  ( 1.035533905932738419, 184.5800000002185186, 9.500000000000003553 ) ) ;
#4364 = CARTESIAN_POINT ( 'NONE',  ( -5.783239563508415948, -1.602707436861142032, 5.973585954366939177 ) ) ;
#4365 = CARTESIAN_POINT ( 'NONE',  ( 1.864425960470169619, 228.0311117417621745, 6.329243341474429130 ) ) ;
#4366 = CARTESIAN_POINT ( 'NONE',  ( 6.105747081304177648, -1.338335777572248420, 5.800265150176761253 ) ) ;
#4367 = CARTESIAN_POINT ( 'NONE',  ( -5.903843691985250608, 2.055287728870591746, 3.999950931234677487 ) ) ;
#4368 = VECTOR ( 'NONE', #6192, 1000.000000000000114 ) ;
#4369 = DIRECTION ( 'NONE',  ( 0.8090169943749506709, -0.5877852522924689183, 0.000000000000000000 ) ) ;
#4370 = ORIENTED_EDGE ( 'NONE', *, *, #11646, .F. ) ;
#4371 = CARTESIAN_POINT ( 'NONE',  ( -0.8561741729129456191, 184.4999999989074979, 4.933012699999999029 ) ) ;
#4372 = PRODUCT_DEFINITION_SHAPE ( 'NONE', 'NONE',  #15315 ) ;
#4373 = CARTESIAN_POINT ( 'NONE',  ( -4.435347140101057128, -4.403429997944487084, 11.49999999999998224 ) ) ;
#4374 = EDGE_LOOP ( 'NONE', ( #2327, #4118, #1098, #589 ) ) ;
#4375 = LINE ( 'NONE', #9446, #12676 ) ;
#4376 = CARTESIAN_POINT ( 'NONE',  ( -5.929230630780102373E-16, 186.2000000000000171, 9.500000000000001776 ) ) ;
#4377 = ADVANCED_FACE ( 'NONE', ( #5040 ), #13612, .F. ) ;
#4378 = AXIS2_PLACEMENT_3D ( 'NONE', #11612, #10505, #6935 ) ;
#4379 = DIRECTION ( 'NONE',  ( 0.9510565162951499785, 0.3090169943749582204, 0.000000000000000000 ) ) ;
#4380 = CARTESIAN_POINT ( 'NONE',  ( -2.782713018890655476, 5.315928322779151394, 31.50439760644212939 ) ) ;
#4381 = CARTESIAN_POINT ( 'NONE',  ( 2.841163418881270886, 5.567120626447992215, 17.73763026556123634 ) ) ;
#4382 = CARTESIAN_POINT ( 'NONE',  ( -1.461580736456473684, 184.7499999989074979, 8.461580736456474128 ) ) ;
#4383 = CARTESIAN_POINT ( 'NONE',  ( -2.931212650151567178, -5.520239928492866710, 5.504259495030093596 ) ) ;
#4384 = EDGE_CURVE ( 'NONE', #7314, #1512, #11023, .T. ) ;
#4385 = CARTESIAN_POINT ( 'NONE',  ( -1.767766952966368432, -1.767766952966369320, 1.100000002184950088 ) ) ;
#4386 = CARTESIAN_POINT ( 'NONE',  ( -6.155854678529475876, -1.081900940642102737, 4.495740504969913509 ) ) ;
#4387 = CARTESIAN_POINT ( 'NONE',  ( 0.000000000000000000, 187.2933328889893687, 9.583808270834989429 ) ) ;
#4388 = CARTESIAN_POINT ( 'NONE',  ( -2.897581130414634077E-17, 9.750000000000003553, 0.000000000000000000 ) ) ;
#4389 = CARTESIAN_POINT ( 'NONE',  ( -5.531209434046278517, -2.328189801702761130, 17.12696220972947714 ) ) ;
#4390 = CARTESIAN_POINT ( 'NONE',  ( -0.8730424326979571159, -5.936362132114481049, 17.49500690218562582 ) ) ;
#4391 = ORIENTED_EDGE ( 'NONE', *, *, #92, .F. ) ;
#4392 = EDGE_CURVE ( 'NONE', #14489, #12984, #11077, .T. ) ;
#4393 = VECTOR ( 'NONE', #2237, 1000.000000000000000 ) ;
#4394 = ORIENTED_EDGE ( 'NONE', *, *, #7177, .T. ) ;
#4395 = ORIENTED_EDGE ( 'NONE', *, *, #792, .T. ) ;
#4396 = CARTESIAN_POINT ( 'NONE',  ( 3.311576095066486314, -5.004818610361370546, 25.47377823943293862 ) ) ;
#4397 = DIRECTION ( 'NONE',  ( 0.000000000000000000, 0.000000000000000000, 1.000000000000000000 ) ) ;
#4398 = ORIENTED_EDGE ( 'NONE', *, *, #5480, .F. ) ;
#4399 = CARTESIAN_POINT ( 'NONE',  ( 2.500000000000000444, 184.8499999999999943, 5.964466094067262247 ) ) ;
#4400 = CARTESIAN_POINT ( 'NONE',  ( 1.035533905932737531, 2.500000000000000444, 1.550000002184949599 ) ) ;
#4401 = CARTESIAN_POINT ( 'NONE',  ( 6.081836621194454118, 1.445163676684769749, 18.87305891554299464 ) ) ;
#4402 = DIRECTION ( 'NONE',  ( -0.000000000000000000, 1.000000000000000000, -0.000000000000000000 ) ) ;
#4403 = CARTESIAN_POINT ( 'NONE',  ( -1.461580736456472795, 185.5499999989075093, 5.538419263543527649 ) ) ;
#4404 = AXIS2_PLACEMENT_3D ( 'NONE', #11699, #3416, #9477 ) ;
#4405 = CARTESIAN_POINT ( 'NONE',  ( 1.035533905932737531, 2.500000000000000444, 1.456999999978150662 ) ) ;
#4406 = DIRECTION ( 'NONE',  ( 0.000000000000000000, 0.000000000000000000, -1.000000000000000000 ) ) ;
#4407 = APPLICATION_PROTOCOL_DEFINITION ( 'draft international standard', 'automotive_design', 1998, #12674 ) ;
#4408 = CARTESIAN_POINT ( 'NONE',  ( 2.066987299999999639, 0.8561741729129456191, 0.1000000010924746996 ) ) ;
#4409 = CARTESIAN_POINT ( 'NONE',  ( 1.767766952966369098, 188.0699999975965397, 5.232233047033630235 ) ) ;
#4410 = CARTESIAN_POINT ( 'NONE',  ( 2.807343268925317492, 227.6302376672054208, 8.330365510804844220 ) ) ;
#4411 = CARTESIAN_POINT ( 'NONE',  ( -0.1960076320828026963, 228.2536001344089982, 10.16376666290868336 ) ) ;
#4412 = ORIENTED_EDGE ( 'NONE', *, *, #6167, .F. ) ;
#4413 = CARTESIAN_POINT ( 'NONE',  ( -1.035533905932738197, -2.500000000000000000, 0.3500000021849497545 ) ) ;
#4414 = VECTOR ( 'NONE', #5011, 1000.000000000000000 ) ;
#4415 = VERTEX_POINT ( 'NONE', #1440 ) ;
#4416 = CARTESIAN_POINT ( 'NONE',  ( -0.6139731865239230757, 6.220476368274060697, 10.69975545601930556 ) ) ;
#4417 = CARTESIAN_POINT ( 'NONE',  ( -1.965116437629976787E-16, 189.6999999978150697, 4.500000000000000000 ) ) ;
#4418 = CARTESIAN_POINT ( 'NONE',  ( 5.558508435838283468, 2.857531096718750607, 24.49999999999999289 ) ) ;
#4419 = EDGE_LOOP ( 'NONE', ( #8309, #10379, #12079, #7755 ) ) ;
#4420 = LINE ( 'NONE', #1941, #12725 ) ;
#4421 = DIRECTION ( 'NONE',  ( 0.000000000000000000, 1.000000000000000000, 0.000000000000000000 ) ) ;
#4422 = CARTESIAN_POINT ( 'NONE',  ( 1.767766952966369320, -1.767766952966368654, 0.3999999999999997446 ) ) ;
#4423 = DIRECTION ( 'NONE',  ( -0.5877852522924685852, -0.8090169943749508930, 0.000000000000000000 ) ) ;
#4424 = DIRECTION ( 'NONE',  ( -1.000000000000000000, 0.000000000000000000, 0.000000000000000000 ) ) ;
#4425 = CARTESIAN_POINT ( 'NONE',  ( -1.050320854595332420E-16, 188.2000000000000171, 4.500000000000000000 ) ) ;
#4426 = CARTESIAN_POINT ( 'NONE',  ( -0.8219475227482178070, 228.8541360017199224, 8.706184346459185264 ) ) ;
#4427 = CARTESIAN_POINT ( 'NONE',  ( 6.081836621194475434, -1.445163676684684484, 17.12694108445698760 ) ) ;
#4428 = DIRECTION ( 'NONE',  ( 0.9510565162951499785, 0.3090169943749582204, 0.000000000000000000 ) ) ;
#4429 = CARTESIAN_POINT ( 'NONE',  ( -1.461580736456472795, 1.461580736456472795, -2.849999998907525089 ) ) ;
#4430 = CARTESIAN_POINT ( 'NONE',  ( 2.500000000000000444, 187.2000000000000171, 7.000000000000000000 ) ) ;
#4431 = CARTESIAN_POINT ( 'NONE',  ( 4.290130679986473794, -4.545972905167823264, 25.11560192892922316 ) ) ;
#4433 = ORIENTED_EDGE ( 'NONE', *, *, #5650, .T. ) ;
#4432 = DIRECTION ( 'NONE',  ( -1.000000000000000000, 0.000000000000000000, 0.000000000000000000 ) ) ;
#4434 = CARTESIAN_POINT ( 'NONE',  ( -5.131373506000823426, 7.062729720843950787, 17.99999999999998934 ) ) ;
#4435 = EDGE_LOOP ( 'NONE', ( #1044, #6479, #2189, #978 ) ) ;
#4436 = ADVANCED_FACE ( 'NONE', ( #11232 ), #12267, .F. ) ;
#4437 = CARTESIAN_POINT ( 'NONE',  ( -5.935543223013858949, 0.8771126767606857166, 31.00000000000000000 ) ) ;
#4438 = CARTESIAN_POINT ( 'NONE',  ( -0.7711655121432159365, 228.2232134260211183, 10.07446308542475499 ) ) ;
#4439 =( NAMED_UNIT ( * ) SI_UNIT ( $, .STERADIAN. ) SOLID_ANGLE_UNIT ( ) );
#4440 = CARTESIAN_POINT ( 'NONE',  ( 6.081836621194470105, 1.445163676684702692, 25.37305891554299819 ) ) ;
#4441 = CARTESIAN_POINT ( 'NONE',  ( -2.500000000000000444, 185.1800000002184561, 8.035533905932737753 ) ) ;
#4442 = CARTESIAN_POINT ( 'NONE',  ( -1.592078987458502848, 227.8601693307692813, 5.835551908609170724 ) ) ;
#4443 = CARTESIAN_POINT ( 'NONE',  ( 1.159630251547017377, 228.7900363578050928, 8.521060918829135744 ) ) ;
#4444 = DIRECTION ( 'NONE',  ( -0.000000000000000000, 1.000000000000000000, -0.000000000000000000 ) ) ;
#4445 = LINE ( 'NONE', #14139, #11092 ) ;
#4446 = CARTESIAN_POINT ( 'NONE',  ( 0.1306171417088810571, 6.000000000000000888, 30.00000000000000000 ) ) ;
#4447 = VERTEX_POINT ( 'NONE', #5195 ) ;
#4448 = CARTESIAN_POINT ( 'NONE',  ( 2.066987299999999639, 189.2999999989075377, 6.143825827087054492 ) ) ;
#4449 = CARTESIAN_POINT ( 'NONE',  ( -0.9740807849835485532, 5.920620690450699719, 11.23850119700668237 ) ) ;
#4450 = EDGE_CURVE ( 'NONE', #15268, #12984, #4574, .T. ) ;
#4451 = ORIENTED_EDGE ( 'NONE', *, *, #15351, .T. ) ;
#4452 = CARTESIAN_POINT ( 'NONE',  ( -4.196038884587126816, -4.289036423669315923, 4.496102049840170700 ) ) ;
#4453 = EDGE_CURVE ( 'NONE', #14180, #14110, #1467, .T. ) ;
#4454 = CARTESIAN_POINT ( 'NONE',  ( 0.8561741729129461742, 185.0999999989074922, 9.066987299999999195 ) ) ;
#4455 = CARTESIAN_POINT ( 'NONE',  ( 3.158296126777706547, 5.394094919772162378, 17.20112161576661691 ) ) ;
#4456 = CARTESIAN_POINT ( 'NONE',  ( 1.461580736456472795, 185.7499999989074979, 8.461580736456474128 ) ) ;
#4457 = CARTESIAN_POINT ( 'NONE',  ( 5.915755444410836006, -1.003187219519639628, 23.99687951097623184 ) ) ;
#4458 = CARTESIAN_POINT ( 'NONE',  ( -1.767766952966369098, 1.767766952966369098, 0.9000000021849497989 ) ) ;
#4459 = CARTESIAN_POINT ( 'NONE',  ( -6.020865209844600052, -1.681180471732124149, 4.025999019766706155 ) ) ;
#4460 = CARTESIAN_POINT ( 'NONE',  ( -5.999999999999999112, 189.3270225533669020, 3.938484906660875584 ) ) ;
#4461 = AXIS2_PLACEMENT_3D ( 'NONE', #4242, #11634, #2973 ) ;
#4462 = CARTESIAN_POINT ( 'NONE',  ( 2.500000000000000444, -1.035533905932737309, 1.250000000000000222 ) ) ;
#4463 = CARTESIAN_POINT ( 'NONE',  ( 4.286401442266577710, -4.198423832313146420, 31.00000000000000000 ) ) ;
#4464 = CARTESIAN_POINT ( 'NONE',  ( 5.931793676715092722, 0.9035324301688769655, 11.76239891805594340 ) ) ;
#4465 = ORIENTED_EDGE ( 'NONE', *, *, #1472, .F. ) ;
#4466 = EDGE_CURVE ( 'NONE', #12035, #11999, #11260, .T. ) ;
#4467 = ORIENTED_EDGE ( 'NONE', *, *, #14690, .F. ) ;
#4468 = ORIENTED_EDGE ( 'NONE', *, *, #6435, .F. ) ;
#4469 = DIRECTION ( 'NONE',  ( 0.000000000000000000, 0.000000000000000000, 1.000000000000000000 ) ) ;
#4470 = CARTESIAN_POINT ( 'NONE',  ( 5.570760634536763511, 2.834026536768326832, 4.737747182782873878 ) ) ;
#4471 = ORIENTED_EDGE ( 'NONE', *, *, #8071, .T. ) ;
#4472 = CARTESIAN_POINT ( 'NONE',  ( -1.767766952966368432, -1.767766952966369320, -0.4999999978150503344 ) ) ;
#4473 = CARTESIAN_POINT ( 'NONE',  ( -5.915653884842702048, -1.003805156977462198, 31.50439760644212939 ) ) ;
#4474 = DIRECTION ( 'NONE',  ( 0.000000000000000000, 0.000000000000000000, -1.000000000000000000 ) ) ;
#4475 = CARTESIAN_POINT ( 'NONE',  ( -2.500000000000000888, 188.2999999978150356, 7.000000000000000000 ) ) ;
#4476 = EDGE_CURVE ( 'NONE', #9576, #10284, #742, .T. ) ;
#4477 = CARTESIAN_POINT ( 'NONE',  ( -1.035533905932738197, -2.500000000000000000, 0.2569999999781503175 ) ) ;
#4478 = B_SPLINE_CURVE_WITH_KNOTS ( 'NONE', 3,
 ( #7915, #903, #5464, #4577, #11800, #3295, #8158, #5617, #5696, #14111, #595, #830, #14036, #12993, #10387, #2019, #11650, #752 ),
 .UNSPECIFIED., .F., .F.,
 ( 4, 2, 2, 2, 2, 2, 2, 2, 4 ),
 ( 0.003131486019302003303, 0.003522824630466707407, 0.003914163241631411945, 0.004305501852796116483, 0.004696840463960820153, 0.005088179075125524690, 0.005479517686290229228, 0.005870856297454934633, 0.006262194908619640038 ),
 .UNSPECIFIED. ) ;
#4479 = CARTESIAN_POINT ( 'NONE',  ( 5.131373506000546314, 7.062729720844130199, 11.49999999999998224 ) ) ;
#4480 = CARTESIAN_POINT ( 'NONE',  ( 0.8561741729129463963, -2.066987299999999195, -0.09999999890752520049 ) ) ;
#4481 = CARTESIAN_POINT ( 'NONE',  ( 4.435347140101073116, -4.403429997944470209, 4.867625892836954904 ) ) ;
#4482 = CARTESIAN_POINT ( 'NONE',  ( 2.990428124265142706, 227.2109326449624120, 7.096232946303270950 ) ) ;
#4483 =( BOUNDED_SURFACE ( )  B_SPLINE_SURFACE ( 1, 2, ( 
 ( #3063, #4257, #592, #5462, #12756, #6658, #4852, #2608, #9627, #8436, #12307, #1332, #5964, #2536, #14379, #3720, #2453, #8597, #4929, #7316, #14545, #13348, #4691, #2370, #8672, #5884, #3642, #64, #1176, #8518, #2288, #11042, #12077, #10731, #7465, #15589, #12156, #6044, #3484, #6205, #4531, #8355, #140, #5005, #9541, #14467, #4769, #13192, #7160, #3566, #7238, #10808, #9858, #14710, #13503, #10966, #11997, #9784, #7389, #10891, #3798, #13272, #1254, #1101, #9708, #15668, #6130, #14630, #13432, #12231, #7621, #1643, #1719, #224, #2849, #12546, #13577, #7539, #5083, #10089, #4115, #1567, #2926, #2768, #451, #10247, #12465, #6363, #12385, #9934, #15022, #4031, #2686, #3872, #7697, #7860, #14786, #1484, #11199, #5160, #299 ),
 ( #8986, #8824, #10014, #8745, #3949, #14861, #13652, #6443, #6519, #11276, #375, #5243, #14939, #13814, #5323, #8906, #13741, #11353, #10167, #7775, #6594, #12622, #11429, #5399, #529, #15098, #4194, #9064, #13890, #3002, #1405, #6280, #11120, #1797, #6907, #9138, #14273, #1875, #15252, #10401, #10322, #4353, #9212, #10553, #14123, #11742, #4272, #5554, #8171, #4591, #11812, #916, #5632, #9287, #6672, #14047, #1954, #3311, #3156, #15409, #12851, #12771, #9362, #681, #4430, #9442, #766, #8011, #2032, #6750, #6829, #7928, #11665, #13011, #10479, #3229, #11505, #15333, #15495, #3383, #8095, #844, #12933, #5709, #13973, #2111, #4507, #606, #12701, #5478, #14203, #6983, #15173, #5786, #10632, #3079, #11583, #8064, #2082, #7111, #14024 ) ),
 .UNSPECIFIED., .F., .F., .F. ) 
 B_SPLINE_SURFACE_WITH_KNOTS ( ( 2, 2 ),
 ( 3, 2, 2, 2, 2, 2, 2, 2, 2, 2, 2, 2, 2, 2, 2, 2, 2, 2, 2, 2, 2, 2, 2, 2, 2, 2, 2, 2, 2, 2, 2, 2, 2, 2, 2, 2, 2, 2, 2, 2, 2, 2, 2, 2, 2, 2, 2, 2, 2, 2, 3 ),
 ( 0.000000000000000000, 1.000000000000000000 ),
 ( 0.000000000000000000, 0.01785714285714285615, 0.03571428571428571230, 0.05357142857142856845, 0.07142857142857142461, 0.08928571428571428770, 0.1071428571428571369, 0.1250000000000000000, 0.1428571428571428492, 0.1607142857142857262, 0.1785714285714285754, 0.1964285714285714246, 0.2142857142857142738, 0.2321428571428571508, 0.2500000000000000000, 0.2678571428571428492, 0.2857142857142856984, 0.3035714285714285476, 0.3214285714285714524, 0.3392857142857143016, 0.3571428571428571508, 0.3750000000000000000, 0.3928571428571428492, 0.4107142857142856984, 0.4285714285714285476, 0.4464285714285714524, 0.4642857142857143016, 0.4821428571428571508, 0.5000000000000000000, 0.5178571428571429047, 0.5357142857142856984, 0.5535714285714286031, 0.5714285714285713969, 0.5892857142857143016, 0.6071428571428570953, 0.6250000000000000000, 0.6428571428571429047, 0.6607142857142856984, 0.6785714285714286031, 0.6964285714285713969, 0.7142857142857143016, 0.7321428571428570953, 0.7500000000000000000, 0.7678571428571429047, 0.7857142857142856984, 0.8035714285714286031, 0.8214285714285713969, 0.8392857142857143016, 0.8571428571428570953, 0.8750000000000000000, 0.8928571428571429047 ),
 .UNSPECIFIED. ) 
 GEOMETRIC_REPRESENTATION_ITEM ( )  RATIONAL_B_SPLINE_SURFACE ( (
 ( 1.000000000000000000, 0.9238795325112867385, 1.000000000000000000, 0.9238795325112867385, 1.000000000000000000, 0.9238795325112867385, 1.000000000000000000, 0.9238795325112867385, 1.000000000000000000, 0.9238795325112867385, 1.000000000000000000, 0.9238795325112867385, 1.000000000000000000, 0.9238795325112867385, 1.000000000000000000, 0.9238795325112867385, 1.000000000000000000, 0.9238795325112867385, 1.000000000000000000, 0.9238795325112867385, 1.000000000000000000, 0.9238795325112867385, 1.000000000000000000, 0.9238795325112867385, 1.000000000000000000, 0.9238795325112867385, 1.000000000000000000, 0.9238795325112867385, 1.000000000000000000, 0.9238795325112867385, 1.000000000000000000, 0.9238795325112867385, 1.000000000000000000, 0.9238795325112867385, 1.000000000000000000, 0.9238795325112867385, 1.000000000000000000, 0.9238795325112867385, 1.000000000000000000, 0.9238795325112867385, 1.000000000000000000, 0.9238795325112867385, 1.000000000000000000, 0.9238795325112867385, 1.000000000000000000, 0.9238795325112867385, 1.000000000000000000, 0.9238795325112867385, 1.000000000000000000, 0.9238795325112867385, 1.000000000000000000, 0.9238795325112867385, 1.000000000000000000, 0.9238795325112867385, 1.000000000000000000, 0.9238795325112867385, 1.000000000000000000, 0.9238795325112867385, 1.000000000000000000, 0.9238795325112867385, 1.000000000000000000, 0.9238795325112867385, 1.000000000000000000, 0.9238795325112867385, 1.000000000000000000, 0.9238795325112867385, 1.000000000000000000, 0.9238795325112867385, 1.000000000000000000, 0.9238795325112867385, 1.000000000000000000, 0.9238795325112867385, 1.000000000000000000, 0.9238795325112867385, 1.000000000000000000, 0.9238795325112867385, 1.000000000000000000, 0.9238795325112867385, 1.000000000000000000, 0.9238795325112867385, 1.000000000000000000, 0.9238795325112867385, 1.000000000000000000, 0.9238795325112867385, 1.000000000000000000, 0.9238795325112867385, 1.000000000000000000, 0.9238795325112867385, 1.000000000000000000, 0.9238795325112867385, 1.000000000000000000, 0.9238795325112867385, 1.000000000000000000, 0.9238795325112867385, 1.000000000000000000, 0.9238795325112867385, 1.000000000000000000, 0.9238795325112867385, 1.000000000000000000, 0.9238795325112867385, 1.000000000000000000),
 ( 1.000000000000000000, 0.9238795325112867385, 1.000000000000000000, 0.9238795325112867385, 1.000000000000000000, 0.9238795325112867385, 1.000000000000000000, 0.9238795325112867385, 1.000000000000000000, 0.9238795325112867385, 1.000000000000000000, 0.9238795325112867385, 1.000000000000000000, 0.9238795325112867385, 1.000000000000000000, 0.9238795325112867385, 1.000000000000000000, 0.9238795325112867385, 1.000000000000000000, 0.9238795325112867385, 1.000000000000000000, 0.9238795325112867385, 1.000000000000000000, 0.9238795325112867385, 1.000000000000000000, 0.9238795325112867385, 1.000000000000000000, 0.9238795325112867385, 1.000000000000000000, 0.9238795325112867385, 1.000000000000000000, 0.9238795325112867385, 1.000000000000000000, 0.9238795325112867385, 1.000000000000000000, 0.9238795325112867385, 1.000000000000000000, 0.9238795325112867385, 1.000000000000000000, 0.9238795325112867385, 1.000000000000000000, 0.9238795325112867385, 1.000000000000000000, 0.9238795325112867385, 1.000000000000000000, 0.9238795325112867385, 1.000000000000000000, 0.9238795325112867385, 1.000000000000000000, 0.9238795325112867385, 1.000000000000000000, 0.9238795325112867385, 1.000000000000000000, 0.9238795325112867385, 1.000000000000000000, 0.9238795325112867385, 1.000000000000000000, 0.9238795325112867385, 1.000000000000000000, 0.9238795325112867385, 1.000000000000000000, 0.9238795325112867385, 1.000000000000000000, 0.9238795325112867385, 1.000000000000000000, 0.9238795325112867385, 1.000000000000000000, 0.9238795325112867385, 1.000000000000000000, 0.9238795325112867385, 1.000000000000000000, 0.9238795325112867385, 1.000000000000000000, 0.9238795325112867385, 1.000000000000000000, 0.9238795325112867385, 1.000000000000000000, 0.9238795325112867385, 1.000000000000000000, 0.9238795325112867385, 1.000000000000000000, 0.9238795325112867385, 1.000000000000000000, 0.9238795325112867385, 1.000000000000000000, 0.9238795325112867385, 1.000000000000000000, 0.9238795325112867385, 1.000000000000000000, 0.9238795325112867385, 1.000000000000000000, 0.9238795325112867385, 1.000000000000000000, 0.9238795325112867385, 1.000000000000000000, 0.9238795325112867385, 1.000000000000000000, 0.9238795325112867385, 1.000000000000000000, 0.9238795325112867385, 1.000000000000000000) ) ) 
 REPRESENTATION_ITEM ( '' )  SURFACE ( )  );
#4484 = EDGE_CURVE ( 'NONE', #5826, #15044, #13204, .T. ) ;
#4485 = CARTESIAN_POINT ( 'NONE',  ( 4.435347140100915020, 4.403429997944631857, 18.13237410716304865 ) ) ;
#4486 = ORIENTED_EDGE ( 'NONE', *, *, #1717, .T. ) ;
#4487 = CARTESIAN_POINT ( 'NONE',  ( 2.668367453516707233, -5.373994336898093138, 5.000000000000004441 ) ) ;
#4488 = ORIENTED_EDGE ( 'NONE', *, *, #2240, .T. ) ;
#4489 = CARTESIAN_POINT ( 'NONE',  ( -0.2622538972263960821, 6.245673238944477568, 12.47385994369196816 ) ) ;
#4490 = CARTESIAN_POINT ( 'NONE',  ( -2.500000000000000888, 189.0999999978150470, 7.000000000000000000 ) ) ;
#4491 = CARTESIAN_POINT ( 'NONE',  ( 5.725930890718356814, 2.506952462183982266, 23.70066851092423832 ) ) ;
#4492 = VERTEX_POINT ( 'NONE', #360 ) ;
#4493 = CARTESIAN_POINT ( 'NONE',  ( -5.783239563508403513, 1.602707436861190438, 17.02641404563305372 ) ) ;
#4494 = CIRCLE ( 'NONE', #5763, 2.499999999999999556 ) ;
#4495 = FACE_BOUND ( 'NONE', #1430, .T. ) ;
#4496 = DIRECTION ( 'NONE',  ( 1.000000000000000000, 0.000000000000000000, 0.000000000000000000 ) ) ;
#4497 = CARTESIAN_POINT ( 'NONE',  ( -2.500000000000000000, 0.000000000000000000, -1.500000000000000000 ) ) ;
#4498 = CARTESIAN_POINT ( 'NONE',  ( -2.692693252389528169, -5.362085866495135633, 31.26382603205595601 ) ) ;
#4499 =( LENGTH_UNIT ( ) NAMED_UNIT ( * ) SI_UNIT ( .MILLI., .METRE. ) );
#4500 = CARTESIAN_POINT ( 'NONE',  ( 0.000000000000000000, 6.250000000000000888, 32.00000000000000000 ) ) ;
#4501 = CARTESIAN_POINT ( 'NONE',  ( -2.500000000000000444, 185.9499999978150413, 8.035533905932737753 ) ) ;
#4502 = CARTESIAN_POINT ( 'NONE',  ( -1.986723294250032357, 228.3028615258686500, 7.114072217564876510 ) ) ;
#4503 = FACE_OUTER_BOUND ( 'NONE', #12060, .T. ) ;
#4504 = CARTESIAN_POINT ( 'NONE',  ( 0.5042675786779833302, 6.230788509548835563, 25.37331068310455251 ) ) ;
#4505 = VECTOR ( 'NONE', #10333, 1000.000000000000000 ) ;
#4506 = CARTESIAN_POINT ( 'NONE',  ( -1.461580736456472351, -1.461580736456473018, -1.049999998907525489 ) ) ;
#4507 = CARTESIAN_POINT ( 'NONE',  ( -1.767766952966369320, 188.2999999999999829, 5.232233047033630235 ) ) ;
#4508 = CARTESIAN_POINT ( 'NONE',  ( -2.500000000000000444, 187.4999999978150527, 7.000000000000000000 ) ) ;
#4510 = VERTEX_POINT ( 'NONE', #5226 ) ;
#4509 = FACE_OUTER_BOUND ( 'NONE', #2810, .T. ) ;
#4511 = CARTESIAN_POINT ( 'NONE',  ( -5.725684683139587783, 2.507514573674819669, 18.79887838423337598 ) ) ;
#4512 = AXIS2_PLACEMENT_3D ( 'NONE', #6569, #11478, #351 ) ;
#4513 = VECTOR ( 'NONE', #6134, 1000.000000000000000 ) ;
#4514 = LINE ( 'NONE', #5486, #10877 ) ;
#4515 = CARTESIAN_POINT ( 'NONE',  ( -2.418857398188632324, 226.7180838673660332, 5.644635841926620934 ) ) ;
#4516 = SHAPE_REPRESENTATION_RELATIONSHIP ( 'NONE' , 'NONE' ,  #13925, #1193 ) ;
#4517 = CARTESIAN_POINT ( 'NONE',  ( -2.500000000000000000, -1.035533905932739307, -0.5499999978150503788 ) ) ;
#4518 = CARTESIAN_POINT ( 'NONE',  ( -1.767766952966369542, 185.2300000002184959, 8.767766952966368876 ) ) ;
#4520 = CARTESIAN_POINT ( 'NONE',  ( -5.842945980534661743, -1.369128644668902384, 5.873784308702619583 ) ) ;
#4519 = B_SPLINE_CURVE_WITH_KNOTS ( 'NONE', 3,
 ( #11287, #14872, #14953, #6455, #384, #5254, #13824, #15031, #310, #7706, #4045, #9075, #540, #2779, #10178, #12631, #2857, #10024, #12710 ),
 .UNSPECIFIED., .F., .F.,
 ( 4, 3, 3, 3, 3, 3, 4 ),
 ( 0.0005593596330526128761, 0.0005760969326736956617, 0.0006092698741508170094, 0.0006292927786811800201, 0.0006633821546468323532, 0.0006974534310236257589, 0.0007078329331167276936 ),
 .UNSPECIFIED. ) ;
#4521 = CARTESIAN_POINT ( 'NONE',  ( 1.078411626687468594, 228.8081072869749732, 8.573250792970148026 ) ) ;
#4522 = FACE_BOUND ( 'NONE', #5283, .T. ) ;
#4523 = CARTESIAN_POINT ( 'NONE',  ( 0.07875310241295396807, 0.4000000000000045186, 2.549923512967463335 ) ) ;
#4524 = DIRECTION ( 'NONE',  ( 0.000000000000000000, 0.000000000000000000, 1.000000000000000000 ) ) ;
#4525 = VERTEX_POINT ( 'NONE', #6264 ) ;
#4526 = CARTESIAN_POINT ( 'NONE',  ( -6.877907531704918753E-16, 189.0499999989075093, 9.066987300000000971 ) ) ;
#4527 = AXIS2_PLACEMENT_3D ( 'NONE', #1741, #6536, #4053 ) ;
#4528 = EDGE_CURVE ( 'NONE', #12751, #13870, #11181, .T. ) ;
#4529 = DIRECTION ( 'NONE',  ( -0.9510565162951544194, 0.3090169943749447312, 0.000000000000000000 ) ) ;
#4530 = AXIS2_PLACEMENT_3D ( 'NONE', #3962, #12476, #1577 ) ;
#4531 = CARTESIAN_POINT ( 'NONE',  ( -2.066987300000000527, 186.2499999989074979, 7.000000000000000000 ) ) ;
#4532 = ORIENTED_EDGE ( 'NONE', *, *, #13034, .T. ) ;
#4533 = B_SPLINE_CURVE_WITH_KNOTS ( 'NONE', 3,
 ( #13076, #13319, #2421, #7289, #2506, #2176, #12125, #6095, #10700, #7362, #1300, #6177, #991, #5855, #11533, #11382, #9092, #3109 ),
 .UNSPECIFIED., .F., .F.,
 ( 4, 2, 2, 2, 2, 2, 2, 2, 4 ),
 ( 0.000000000000000000, 0.0003914904498596253886, 0.0007829808997192507771, 0.001174471349578876112, 0.001565961799438501554, 0.001957452249298126997, 0.002348942699157752223, 0.002740433149017377883, 0.003131923598877003109 ),
 .UNSPECIFIED. ) ;
#4534 = CARTESIAN_POINT ( 'NONE',  ( -3.107688324358628407, -5.133887830459884505, 4.126215691297385746 ) ) ;
#4535 = DIRECTION ( 'NONE',  ( 0.000000000000000000, 0.000000000000000000, -1.000000000000000000 ) ) ;
#4536 = CARTESIAN_POINT ( 'NONE',  ( 5.317509234263996021, 2.779225709350927609, 17.86760611998364823 ) ) ;
#4537 = CARTESIAN_POINT ( 'NONE',  ( 0.8561741729129457301, 185.1999999989075434, 4.933012699999999029 ) ) ;
#4538 = VECTOR ( 'NONE', #1294, 1000.000000000000000 ) ;
#4539 = CARTESIAN_POINT ( 'NONE',  ( -2.817313151351109379, -5.579000502529471994, 5.000000000000004441 ) ) ;
#4540 = CARTESIAN_POINT ( 'NONE',  ( -1.035533905932738197, -2.500000000000000000, -1.249999997815050223 ) ) ;
#4541 = DIRECTION ( 'NONE',  ( -0.000000000000000000, 1.000000000000000000, -0.000000000000000000 ) ) ;
#4542 = CARTESIAN_POINT ( 'NONE',  ( 3.659182332138577465E-16, 227.2817795252328210, 4.165129161027028459 ) ) ;
#4543 = CARTESIAN_POINT ( 'NONE',  ( -2.500000000000000000, 0.000000000000000000, -2.300000000000000266 ) ) ;
#4544 = CARTESIAN_POINT ( 'NONE',  ( -1.265664690411614835E-16, 2.066987299999999639, -1.949999998907525622 ) ) ;
#4545 = CARTESIAN_POINT ( 'NONE',  ( -2.897581130414634077E-17, 22.00000000000000000, -9.750000000000003553 ) ) ;
#4546 = ADVANCED_FACE ( 'NONE', ( #14923 ), #13724, .F. ) ;
#4547 = EDGE_LOOP ( 'NONE', ( #15309, #13295 ) ) ;
#4548 = EDGE_CURVE ( 'NONE', #8273, #1022, #9605, .T. ) ;
#4549 = ORIENTED_EDGE ( 'NONE', *, *, #877, .F. ) ;
#4550 =( REPRESENTATION_RELATIONSHIP ('NONE','NONE', #11191, #3059 ) REPRESENTATION_RELATIONSHIP_WITH_TRANSFORMATION ( #14248 )SHAPE_REPRESENTATION_RELATIONSHIP( ) );
#4551 = AXIS2_PLACEMENT_3D ( 'NONE', #12645, #10268, #3101 ) ;
#4552 = ORIENTED_EDGE ( 'NONE', *, *, #1709, .T. ) ;
#4553 = CARTESIAN_POINT ( 'NONE',  ( 2.066987300000000083, 185.2999999989075661, 6.143825827087054492 ) ) ;
#4554 = CARTESIAN_POINT ( 'NONE',  ( 1.990438725498679062, 228.3461478020684865, 7.239085452117288710 ) ) ;
#4555 = EDGE_CURVE ( 'NONE', #12950, #12135, #3296, .T. ) ;
#4556 = ORIENTED_EDGE ( 'NONE', *, *, #2168, .T. ) ;
#4557 = B_SPLINE_CURVE_WITH_KNOTS ( 'NONE', 3,
 ( #13773, #6401, #11233, #10355, #4308, #9170, #3985, #335, #5196, #1757, #6552, #2882, #12502, #7729, #1677, #10204, #9021, #12660 ),
 .UNSPECIFIED., .F., .F.,
 ( 4, 2, 2, 2, 2, 2, 2, 2, 4 ),
 ( 0.000000000000000000, 0.0003914362731607569780, 0.0007828725463215139560, 0.001174308819482270880, 0.001565745092643027912, 0.001957181365803784944, 0.002348617638964541759, 0.002740053912125299009, 0.003131490185286055824 ),
 .UNSPECIFIED. ) ;
#4558 = CARTESIAN_POINT ( 'NONE',  ( 4.435347140100928343, -4.403429997944614982, 24.49999999999999289 ) ) ;
#4559 = CARTESIAN_POINT ( 'NONE',  ( 2.996417732210394647, 5.485687819087000427, 25.11396179408070850 ) ) ;
#4560 = CARTESIAN_POINT ( 'NONE',  ( 2.066987300000000083, 185.2999999989075377, 6.143825827087054492 ) ) ;
#4561 = CARTESIAN_POINT ( 'NONE',  ( -1.035533905932738197, -2.500000000000000000, -1.343000000021849383 ) ) ;
#4562 = CARTESIAN_POINT ( 'NONE',  ( -4.435347140101218777, 4.403429997944323659, 24.49999999999999289 ) ) ;
#4563 = COLOUR_RGB ( '', 0.08235294, 0.09019608, 0.10196078) ;
#4564 = CARTESIAN_POINT ( 'NONE',  ( 2.066987300000000083, -0.8561741729129449530, 1.092474635061568626E-09 ) ) ;
#4565 = CARTESIAN_POINT ( 'NONE',  ( -1.767766952966369320, 188.2699999975965568, 5.232233047033630235 ) ) ;
#4566 = CARTESIAN_POINT ( 'NONE',  ( -0.9651034952757481244, 226.3762748196293728, 4.637298184581183591 ) ) ;
#4567 = CARTESIAN_POINT ( 'NONE',  ( -12.50000000000000533, 0.000000000000000000, 2.000000000000001776 ) ) ;
#4568 = ORIENTED_EDGE ( 'NONE', *, *, #9396, .T. ) ;
#4569 = CARTESIAN_POINT ( 'NONE',  ( -5.375605342016444688, 2.665598297262417482, 25.00312048902378237 ) ) ;
#4570 = ORIENTED_EDGE ( 'NONE', *, *, #15674, .F. ) ;
#4571 = CARTESIAN_POINT ( 'NONE',  ( -5.648794263291700979, 2.676232015153707344, 25.11441947245483064 ) ) ;
#4572 = SURFACE_STYLE_USAGE ( .BOTH. , #15474 ) ;
#4573 =( GEOMETRIC_REPRESENTATION_CONTEXT ( 3 ) GLOBAL_UNCERTAINTY_ASSIGNED_CONTEXT ( ( #12199 ) ) GLOBAL_UNIT_ASSIGNED_CONTEXT ( ( #12535, #4107, #11344 ) ) REPRESENTATION_CONTEXT ( 'NONE', 'WORKASPACE' ) );
#4574 = B_SPLINE_CURVE_WITH_KNOTS ( 'NONE', 3,
 ( #6318, #6240, #11155, #257, #13694, #13539, #7500, #2804, #12501, #13464, #14746, #8782, #1600, #1367, #3832, #3856, #2590, #1628 ),
 .UNSPECIFIED., .F., .F.,
 ( 4, 2, 2, 2, 2, 2, 2, 2, 4 ),
 ( 0.000000000000000000, 0.0003914357524127485156, 0.0007828715048254970311, 0.001174307257238245547, 0.001565743009650994062, 0.001957178762063742361, 0.002348614514476491093, 0.002740050266889239826, 0.003131486019301988125 ),
 .UNSPECIFIED. ) ;
#4575 = DIRECTION ( 'NONE',  ( -0.000000000000000000, -1.000000000000000000, -0.000000000000000000 ) ) ;
#4576 = ORIENTED_EDGE ( 'NONE', *, *, #13999, .T. ) ;
#4577 = CARTESIAN_POINT ( 'NONE',  ( 2.930600586412910324, 5.520563544161783298, 10.99691356133952169 ) ) ;
#4578 = CARTESIAN_POINT ( 'NONE',  ( 5.621197618055753686, -2.101623592078309510, 17.02601979877759319 ) ) ;
#4579 = CARTESIAN_POINT ( 'NONE',  ( 0.000000000000000000, 19.99999999999999645, 0.000000000000000000 ) ) ;
#4580 = CARTESIAN_POINT ( 'NONE',  ( -3.883588957979267065, -4.898466244118923285, 18.97377282875267923 ) ) ;
#4581 = CARTESIAN_POINT ( 'NONE',  ( 1.767766952966368654, 1.767766952966369098, 0.6000000000000000888 ) ) ;
#4582 = CARTESIAN_POINT ( 'NONE',  ( -3.011385983131315225, -5.190390249166442871, 31.79952054102716374 ) ) ;
#4583 = FILL_AREA_STYLE ('',( #9279 ) ) ;
#4584 = FACE_OUTER_BOUND ( 'NONE', #8867, .T. ) ;
#4585 = ADVANCED_FACE ( 'NONE', ( #12450 ), #6426, .F. ) ;
#4586 = CARTESIAN_POINT ( 'NONE',  ( -1.767766952966369542, 185.9999999978150527, 8.767766952966368876 ) ) ;
#4587 = CARTESIAN_POINT ( 'NONE',  ( 0.9648499430152943646, 228.2043505555869274, 10.01897217821435859 ) ) ;
#4588 = CARTESIAN_POINT ( 'NONE',  ( -5.558508435838126260, -2.857531096719055697, 18.13063932754212004 ) ) ;
#4589 = CARTESIAN_POINT ( 'NONE',  ( -2.251711471503315298, 189.9958096512905286, 5.235413736675446295 ) ) ;
#4590 = EDGE_CURVE ( 'NONE', #7332, #5826, #10384, .T. ) ;
#4591 = CARTESIAN_POINT ( 'NONE',  ( 2.500000000000000444, 186.4500000000000171, 5.964466094067262247 ) ) ;
#4592 = CARTESIAN_POINT ( 'NONE',  ( -4.267838854167155027, 4.217593933790356964, 4.737601081944045056 ) ) ;
#4594 = VERTEX_POINT ( 'NONE', #9271 ) ;
#4593 = CARTESIAN_POINT ( 'NONE',  ( 2.500000000000000000, 3.061616997868383141E-16, -1.799999997815050490 ) ) ;
#4595 = CARTESIAN_POINT ( 'NONE',  ( -5.903061651806585708, 2.057626436184840646, 18.99991741810287493 ) ) ;
#4596 = SHAPE_REPRESENTATION ( 'slotted cheese head screw_iso_ISO 1207 - M3 x 5 - 5N', ( #14201 ), #3292 ) ;
#4597 = CARTESIAN_POINT ( 'NONE',  ( -6.776263578034402713E-18, 186.5999999999999943, 4.500000000000000000 ) ) ;
#4598 = CARTESIAN_POINT ( 'NONE',  ( -2.791088703906231760, 226.9357700049156108, 6.285935106528314442 ) ) ;
#4599 = SHAPE_REPRESENTATION_RELATIONSHIP ( 'NONE' , 'NONE' ,  #11283, #8222 ) ;
#4600 = CARTESIAN_POINT ( 'NONE',  ( 5.649200442566227665, 2.675373855294000514, 25.11560192892921606 ) ) ;
#4601 = CARTESIAN_POINT ( 'NONE',  ( 1.035533905932737975, 184.8800000002185016, 4.500000000000000888 ) ) ;
#4602 = CARTESIAN_POINT ( 'NONE',  ( 0.000000000000000000, 0.000000000000000000, 2.500000000000000000 ) ) ;
#4603 = CARTESIAN_POINT ( 'NONE',  ( 0.9944270131901197241, 228.8248696211178981, 8.621661370035813121 ) ) ;
#4604 = FACE_BOUND ( 'NONE', #9002, .T. ) ;
#4605 = CARTESIAN_POINT ( 'NONE',  ( -1.265664690411614835E-16, 2.066987299999999639, 0.4500000010924747329 ) ) ;
#4606 = CARTESIAN_POINT ( 'NONE',  ( -4.286401442266531525, -4.198423832313195270, 5.000000000000004441 ) ) ;
#4607 = ORIENTED_EDGE ( 'NONE', *, *, #7801, .F. ) ;
#4608 = CARTESIAN_POINT ( 'NONE',  ( 0.09128442572522987852, 0.000000000000000000, 0.000000000000000000 ) ) ;
#4609 =( BOUNDED_CURVE ( )  B_SPLINE_CURVE ( 2, ( #13664, #7399, #5094, #12241, #14951, #6217, #9945, #11052, #1575 ),
 .UNSPECIFIED., .F., .F. ) 
 B_SPLINE_CURVE_WITH_KNOTS ( ( 3, 2, 2, 2, 3 ),
 ( 0.3571428571428571508, 0.3750000000000000000, 0.3928571428571428492, 0.4107142857142856984, 0.4285714285714285476 ),
 .UNSPECIFIED. ) 
 CURVE ( )  GEOMETRIC_REPRESENTATION_ITEM ( )  RATIONAL_B_SPLINE_CURVE ( ( 1.000000000000000000, 0.9238795325112867385, 1.000000000000000000, 0.9238795325112867385, 1.000000000000000000, 0.9238795325112867385, 1.000000000000000000, 0.9238795325112867385, 1.000000000000000000 ) ) 
 REPRESENTATION_ITEM ( '' )  );
#4610 = CARTESIAN_POINT ( 'NONE',  ( -8.666684749742561339E-31, 189.0000000000000000, 4.500000000000000888 ) ) ;
#4611 = ORIENTED_EDGE ( 'NONE', *, *, #9756, .F. ) ;
#4612 = DIRECTION ( 'NONE',  ( -1.000000000000000000, 3.326610055774643275E-18, -1.062480551894329622E-17 ) ) ;
#4613 = ADVANCED_BREP_SHAPE_REPRESENTATION ( '', ( #10345, #14201 ), #13708 ) ;
#4614 = CARTESIAN_POINT ( 'NONE',  ( 0.000000000000000000, 0.000000000000000000, 5.000000000000004441 ) ) ;
#4615 = CARTESIAN_POINT ( 'NONE',  ( 5.317509234263995133, 2.779225709350928053, 17.99999999999998934 ) ) ;
#4616 = CARTESIAN_POINT ( 'NONE',  ( -2.066987300000000527, 185.4499999989075150, 7.000000000000000000 ) ) ;
#4617 = CARTESIAN_POINT ( 'NONE',  ( 3.632753594129368047, -4.777047695050953280, 30.00004946353777768 ) ) ;
#4618 = CARTESIAN_POINT ( 'NONE',  ( 4.592425496802573972E-16, -2.500000000000000000, -1.199999997815050179 ) ) ;
#4619 = CYLINDRICAL_SURFACE ( 'NONE', #13150, 1.499999999999999556 ) ;
#4620 = CARTESIAN_POINT ( 'NONE',  ( -5.999999999999999112, 215.7452399395091618, 13.29567785264566027 ) ) ;
#4621 = CARTESIAN_POINT ( 'NONE',  ( 0.9735954530125449091, -6.173909381473989377, 31.26281793585245694 ) ) ;
#4622 = CARTESIAN_POINT ( 'NONE',  ( 2.999999999999999556, 1.732050807568877859, -5.500000000000000000 ) ) ;
#4623 = CARTESIAN_POINT ( 'NONE',  ( 0.000000000000000000, 189.6977690162252657, 10.38967773564543862 ) ) ;
#4624 = VERTEX_POINT ( 'NONE', #826 ) ;
#4625 = VERTEX_POINT ( 'NONE', #11797 ) ;
#4626 = VERTEX_POINT ( 'NONE', #3212 ) ;
#4627 = VECTOR ( 'NONE', #2522, 1000.000000000000000 ) ;
#4628 = CARTESIAN_POINT ( 'NONE',  ( 2.996920846510496172, 5.485395142346785491, 30.38558052754516225 ) ) ;
#4629 = CARTESIAN_POINT ( 'NONE',  ( -4.196038884587224516, 4.289036423669218223, 12.00389795015984973 ) ) ;
#4630 = VERTEX_POINT ( 'NONE', #6734 ) ;
#4631 = CARTESIAN_POINT ( 'NONE',  ( -2.066987299999999639, 0.8561741729129452860, 2.000000001092474555 ) ) ;
#4632 = EDGE_CURVE ( 'NONE', #4630, #12887, #12834, .T. ) ;
#4633 = CARTESIAN_POINT ( 'NONE',  ( 2.031800924177950305E-13, 6.000000000000000888, 23.49999999999999289 ) ) ;
#4634 = CARTESIAN_POINT ( 'NONE',  ( 0.000000000000000000, 0.000000000000000000, 5.000000000000004441 ) ) ;
#4635 = CARTESIAN_POINT ( 'NONE',  ( -5.895349312889930360E-16, 187.4499999989075150, 9.066987300000000971 ) ) ;
#4636 = CARTESIAN_POINT ( 'NONE',  ( -2.500000000000000444, 1.035533905932737753, -1.543000000021849338 ) ) ;
#4637 = ADVANCED_FACE ( 'NONE', ( #7912 ), #10614, .F. ) ;
#4638 = CARTESIAN_POINT ( 'NONE',  ( 2.500000000000000444, 185.5499999978150356, 5.964466094067262247 ) ) ;
#4639 = CARTESIAN_POINT ( 'NONE',  ( 1.461580736456472573, 1.461580736456472795, -0.6499999989075253559 ) ) ;
#4640 = AXIS2_PLACEMENT_3D ( 'NONE', #11069, #13371, #2481 ) ;
#4641 = DIRECTION ( 'NONE',  ( -0.5877852522924685852, -0.8090169943749507819, 0.000000000000000000 ) ) ;
#4642 = CARTESIAN_POINT ( 'NONE',  ( 1.328920255623610380, 226.4243263863947391, 4.778947530392284371 ) ) ;
#4643 = B_SPLINE_CURVE_WITH_KNOTS ( 'NONE', 3,
 ( #2633, #11064, #7563, #322, #1588, #1510, #11143, #10037, #7487, #6385, #1275, #6466, #13367, #9730, #12332, #163, #5026, #14568 ),
 .UNSPECIFIED., .F., .F.,
 ( 4, 2, 2, 2, 2, 2, 2, 2, 4 ),
 ( 0.000000000000000000, 0.0003914898357794973326, 0.0007829796715589946651, 0.001174469507338491998, 0.001565959343117989330, 0.001957449178897486663, 0.002348939014676983995, 0.002740428850456481328, 0.003131918686235978661 ),
 .UNSPECIFIED. ) ;
#4644 = CARTESIAN_POINT ( 'NONE',  ( -1.748661130334981051, 228.0746845563984095, 9.637707355516731411 ) ) ;
#4645 = VERTEX_POINT ( 'NONE', #15158 ) ;
#4646 = ORIENTED_EDGE ( 'NONE', *, *, #11914, .T. ) ;
#4647 = CARTESIAN_POINT ( 'NONE',  ( 2.668367453516705901, -5.373994336898094915, 4.869350386511452911 ) ) ;
#4648 = VERTEX_POINT ( 'NONE', #9193 ) ;
#4649 = EDGE_LOOP ( 'NONE', ( #1506, #1330 ) ) ;
#4650 = CARTESIAN_POINT ( 'NONE',  ( 0.2637975869347874425, 6.245592211692893692, 31.97332839949191552 ) ) ;
#4651 = EDGE_CURVE ( 'NONE', #7968, #9805, #6812, .T. ) ;
#4652 = CARTESIAN_POINT ( 'NONE',  ( 3.922288969639753375, -4.542045818322549167, 17.12621569129736798 ) ) ;
#4653 = CARTESIAN_POINT ( 'NONE',  ( 0.9735954530125295880, -6.173909381473990265, 5.262817935852433848 ) ) ;
#4654 = ORIENTED_EDGE ( 'NONE', *, *, #14129, .F. ) ;
#4655 = CARTESIAN_POINT ( 'NONE',  ( -6.020865209844618704, 1.681180471732060422, 31.97400098023329917 ) ) ;
#4656 = EDGE_CURVE ( 'NONE', #8072, #8675, #3062, .T. ) ;
#4657 = CARTESIAN_POINT ( 'NONE',  ( 6.123233995736766282E-16, -6.250000000000000888, 6.000000000000005329 ) ) ;
#4658 = B_SPLINE_CURVE_WITH_KNOTS ( 'NONE', 3,
 ( #8574, #11440, #9076, #3240, #5567, #15109, #4520, #4364, #10413, #7786, #10564, #11752, #13825, #778, #11516, #9149, #6682, #3013 ),
 .UNSPECIFIED., .F., .F.,
 ( 4, 2, 2, 2, 2, 2, 2, 2, 4 ),
 ( 0.000000000000000000, 0.0003914898357794940800, 0.0007829796715589883768, 0.001174469507338482457, 0.001565959343117977187, 0.001957449178897471484, 0.002348939014676964913, 0.002740428850456459210, 0.003131918686235953507 ),
 .UNSPECIFIED. ) ;
#4659 = CARTESIAN_POINT ( 'NONE',  ( -0.9740012993918163442, -6.173846968979670891, 24.76164920628438182 ) ) ;
#4660 = CARTESIAN_POINT ( 'NONE',  ( 1.734723475976807094E-15, -0.001000000000000132727, 15.50000000000000000 ) ) ;
#4661 = CARTESIAN_POINT ( 'NONE',  ( -5.725684683139530051, -2.507514573674952452, 23.70112161576660625 ) ) ;
#4662 = CARTESIAN_POINT ( 'NONE',  ( -3.781065399486090328, -4.978303713186380541, 25.49991741810288204 ) ) ;
#4663 = DIRECTION ( 'NONE',  ( 1.000000000000000000, 0.000000000000000000, 0.000000000000000000 ) ) ;
#4664 = CARTESIAN_POINT ( 'NONE',  ( 2.500000000000000444, 189.5499999978150640, 5.964466094067262247 ) ) ;
#4665 = CARTESIAN_POINT ( 'NONE',  ( 1.707343418157801551, 228.0835877007203294, 9.663887492166837845 ) ) ;
#4666 = CARTESIAN_POINT ( 'NONE',  ( -5.903843691985178666, -2.055287728870804909, 19.00004906876531408 ) ) ;
#4667 = CARTESIAN_POINT ( 'NONE',  ( -11.25000000000000355, 3.419666426228851687E-14, 0.000000000000000000 ) ) ;
#4668 = VERTEX_POINT ( 'NONE', #9124 ) ;
#4669 = CARTESIAN_POINT ( 'NONE',  ( -5.486741141153783197, 2.429871531109751182, 12.29888242247938202 ) ) ;
#4670 = DIRECTION ( 'NONE',  ( 1.000000000000000000, 0.000000000000000000, 0.000000000000000000 ) ) ;
#4672 = ORIENTED_EDGE ( 'NONE', *, *, #8274, .F. ) ;
#4671 = CARTESIAN_POINT ( 'NONE',  ( -2.817313151351169775, -5.579000502529442684, 11.49999999999998224 ) ) ;
#4673 = CARTESIAN_POINT ( 'NONE',  ( 0.09128442572411965550, -0.3999999999999975797, 2.551849451881568420 ) ) ;
#4674 = CARTESIAN_POINT ( 'NONE',  ( 2.244217608389459162, 226.6470584425424306, 5.435389493528692384 ) ) ;
#4675 = EDGE_LOOP ( 'NONE', ( #15609, #4772, #7024, #14824 ) ) ;
#4676 = CARTESIAN_POINT ( 'NONE',  ( 6.250000000000000888, 7.654042494670958593E-16, 36.00000000000000711 ) ) ;
#4677 = CARTESIAN_POINT ( 'NONE',  ( -0.8561741729129455081, 2.066987299999999639, -0.2999999989075253226 ) ) ;
#4678 = CARTESIAN_POINT ( 'NONE',  ( -2.882630993546674070, 227.5642217159421818, 8.136181965847606889 ) ) ;
#4679 =( NAMED_UNIT ( * ) SI_UNIT ( $, .STERADIAN. ) SOLID_ANGLE_UNIT ( ) );
#4680 = EDGE_CURVE ( 'NONE', #10824, #3215, #900, .T. ) ;
#4681 = CARTESIAN_POINT ( 'NONE',  ( 0.4899822127396957772, 190.0840757508179593, 4.235790927168524789 ) ) ;
#4682 = CARTESIAN_POINT ( 'NONE',  ( -1.767766952966369320, 185.8300000002185186, 5.232233047033630235 ) ) ;
#4683 = CARTESIAN_POINT ( 'NONE',  ( -3.000000000000000000, 1.732050807568877415, -5.500000000000000000 ) ) ;
#4684 = CARTESIAN_POINT ( 'NONE',  ( -1.965306002007385144, 228.1545512627131131, 6.685743718507844768 ) ) ;
#4685 = FACE_BOUND ( 'NONE', #751, .T. ) ;
#4686 = CARTESIAN_POINT ( 'NONE',  ( -1.265664690411614835E-16, 2.066987299999999639, 1.250000001092474777 ) ) ;
#4687 = CARTESIAN_POINT ( 'NONE',  ( 1.000079958708160355, 5.916066267613696361, 31.13152738882034143 ) ) ;
#4688 = EDGE_CURVE ( 'NONE', #4232, #5611, #6965, .T. ) ;
#4689 = ORIENTED_EDGE ( 'NONE', *, *, #12602, .F. ) ;
#4690 = CARTESIAN_POINT ( 'NONE',  ( 2.066987300000000971, 187.4999999989075548, 6.143825827087054492 ) ) ;
#4691 = CARTESIAN_POINT ( 'NONE',  ( -1.461580736456473018, 185.3499999989074922, 5.538419263543526760 ) ) ;
#4692 = CARTESIAN_POINT ( 'NONE',  ( -4.154121946520892728, -4.670585111242955278, 12.29887838423337953 ) ) ;
#4693 = ORIENTED_EDGE ( 'NONE', *, *, #9405, .T. ) ;
#4694 =( BOUNDED_CURVE ( )  B_SPLINE_CURVE ( 2, ( #13313, #31, #7122, #2253, #2170, #11874, #9752, #14590, #3686 ),
 .UNSPECIFIED., .F., .F. ) 
 B_SPLINE_CURVE_WITH_KNOTS ( ( 3, 2, 2, 2, 3 ),
 ( 0.2142857142857143293, 0.2321428571428572063, 0.2500000000000000000, 0.2678571428571428492, 0.2857142857142856984 ),
 .UNSPECIFIED. ) 
 CURVE ( )  GEOMETRIC_REPRESENTATION_ITEM ( )  RATIONAL_B_SPLINE_CURVE ( ( 0.9999999999999997780, 0.9238795325112869605, 1.000000000000000000, 0.9238795325112867385, 1.000000000000000000, 0.9238795325112867385, 1.000000000000000000, 0.9238795325112867385, 1.000000000000000000 ) ) 
 REPRESENTATION_ITEM ( '' )  );
#4695 = CARTESIAN_POINT ( 'NONE',  ( -3.922672396097006242, -4.541739265057743502, 4.126352953155773662 ) ) ;
#4696 = FACE_OUTER_BOUND ( 'NONE', #12094, .T. ) ;
#4697 = CARTESIAN_POINT ( 'NONE',  ( -2.849269941562008857, 5.281123252784022171, 31.61519382448851090 ) ) ;
#4698 = CARTESIAN_POINT ( 'NONE',  ( 0.1306070469494091113, 6.249999999999999112, 10.49999999999998401 ) ) ;
#4699 = CARTESIAN_POINT ( 'NONE',  ( -5.793705359219414319E-16, 187.2499999989075263, 9.066987300000000971 ) ) ;
#4700 = CARTESIAN_POINT ( 'NONE',  ( 3.107278289587086739, 5.134157760522114700, 18.87364704684421923 ) ) ;
#4701 = CARTESIAN_POINT ( 'NONE',  ( -1.767766952966368432, -1.767766952966369320, -1.299999997815050490 ) ) ;
#4702 = CARTESIAN_POINT ( 'NONE',  ( -6.142844459177239536, -1.156093792145200361, 4.384398071070797265 ) ) ;
#4703 = CARTESIAN_POINT ( 'NONE',  ( 1.035533905932737975, 184.1499999999999773, 4.500000000000001776 ) ) ;
#4704 = CARTESIAN_POINT ( 'NONE',  ( 1.035533905932737753, 188.8499999978150186, 4.500000000000001776 ) ) ;
#4705 = CARTESIAN_POINT ( 'NONE',  ( -5.558508435838199091, 2.857531096718913588, 11.36936067245786397 ) ) ;
#4706 = CARTESIAN_POINT ( 'NONE',  ( -0.06431340346706571065, 189.6978264018315770, 10.38900192207087336 ) ) ;
#4707 = CIRCLE ( 'NONE', #13582, 2.483389555546411831 ) ;
#4708 = EDGE_LOOP ( 'NONE', ( #6912, #13048 ) ) ;
#4709 = EDGE_LOOP ( 'NONE', ( #5435, #4132 ) ) ;
#4710 = ORIENTED_EDGE ( 'NONE', *, *, #4181, .T. ) ;
#4711 = CARTESIAN_POINT ( 'NONE',  ( 1.728762592943754006, 227.9346299510661140, 6.050598426982102040 ) ) ;
#4712 = EDGE_LOOP ( 'NONE', ( #8669, #10210, #264, #4313 ) ) ;
#4713 = CARTESIAN_POINT ( 'NONE',  ( -2.500000000000000000, 0.000000000000000000, -2.199999997815050623 ) ) ;
#4714 = CARTESIAN_POINT ( 'NONE',  ( -5.666074146197994210, -1.978051345703167208, 32.00004932073311892 ) ) ;
#4715 = AXIS2_PLACEMENT_3D ( 'NONE', #907, #11880, #15400 ) ;
#4716 = CARTESIAN_POINT ( 'NONE',  ( 5.558508435838199979, 2.857531096718914476, 31.00000000000000000 ) ) ;
#4717 = CARTESIAN_POINT ( 'NONE',  ( -0.8561741729129469514, 188.1999999989075150, 9.066987299999999195 ) ) ;
#4718 = CARTESIAN_POINT ( 'NONE',  ( 2.500000000000000000, 3.061616997868383141E-16, -0.2930000000218493938 ) ) ;
#4719 = LINE ( 'NONE', #2005, #15317 ) ;
#4720 = EDGE_CURVE ( 'NONE', #5689, #2728, #246, .T. ) ;
#4721 = CONTEXT_DEPENDENT_SHAPE_REPRESENTATION ( #198, #14016 ) ;
#4722 = CARTESIAN_POINT ( 'NONE',  ( -2.066987299999999639, 0.000000000000000000, -1.949999998907525178 ) ) ;
#4723 = CARTESIAN_POINT ( 'NONE',  ( 3.254737477228057951, -5.337033878705167211, 30.12632671364006143 ) ) ;
#4724 = CARTESIAN_POINT ( 'NONE',  ( -0.7768053109583262783, 226.3575155338836282, 4.581995736916623763 ) ) ;
#4725 = DIRECTION ( 'NONE',  ( 0.000000000000000000, 0.000000000000000000, 1.000000000000000000 ) ) ;
#4726 = ORIENTED_EDGE ( 'NONE', *, *, #14352, .F. ) ;
#4727 = EDGE_LOOP ( 'NONE', ( #6809, #1118 ) ) ;
#4728 = B_SPLINE_CURVE_WITH_KNOTS ( 'NONE', 3,
 ( #1299, #9907, #13476, #6176, #2578, #190, #6415, #14761, #349, #8718, #5213, #6333, #7824, #6721, #5448, #9111, #10142, #13861 ),
 .UNSPECIFIED., .F., .F.,
 ( 4, 2, 2, 2, 2, 2, 2, 2, 4 ),
 ( 0.000000000000000000, 0.0003914898357794969531, 0.0007829796715589939062, 0.001174469507338490913, 0.001565959343117987812, 0.001957449178897484928, 0.002348939014676981827, 0.002740428850456478726, 0.003131918686235975625 ),
 .UNSPECIFIED. ) ;
#4729 = DIRECTION ( 'NONE',  ( -0.9510565162951544194, 0.3090169943749447312, 0.000000000000000000 ) ) ;
#4730 = VERTEX_POINT ( 'NONE', #5537 ) ;
#4731 = ORIENTED_EDGE ( 'NONE', *, *, #11819, .T. ) ;
#4732 = EDGE_CURVE ( 'NONE', #7444, #6574, #2468, .T. ) ;
#4733 = CARTESIAN_POINT ( 'NONE',  ( -5.903061651806561727, 2.057626436184907703, 25.49991741810288559 ) ) ;
#4734 = CARTESIAN_POINT ( 'NONE',  ( -4.070051655338184915, -4.744673454622407860, 23.62632671364005432 ) ) ;
#4735 = CARTESIAN_POINT ( 'NONE',  ( 0.6139731865239909103, -6.220476368274053591, 4.199755456019331312 ) ) ;
#4736 = CARTESIAN_POINT ( 'NONE',  ( -5.984595133899166974, -1.806709459528702988, 31.99995078984293428 ) ) ;
#4737 = CARTESIAN_POINT ( 'NONE',  ( -0.9737725088282169761, -6.173885267451821868, 4.737357587265639935 ) ) ;
#4738 = CARTESIAN_POINT ( 'NONE',  ( 0.000000000000000000, 0.000000000000000000, 2.000000000000001776 ) ) ;
#4739 = CYLINDRICAL_SURFACE ( 'NONE', #10811, 5.000000000000000000 ) ;
#4740 = CARTESIAN_POINT ( 'NONE',  ( 5.620786884546272510, 2.102685372472933967, 30.02641404563307148 ) ) ;
#4741 = CARTESIAN_POINT ( 'NONE',  ( -1.084202172485504434E-16, 3.464101615137754830, -5.500000000000000000 ) ) ;
#4742 = DIRECTION ( 'NONE',  ( -1.000000000000000000, 0.000000000000000000, -3.491481338843133355E-15 ) ) ;
#4743 = CARTESIAN_POINT ( 'NONE',  ( -1.035533905932737975, 188.1499999978150868, 4.500000000000000888 ) ) ;
#4744 = CARTESIAN_POINT ( 'NONE',  ( 2.990428124265142706, 227.2109326449624120, 7.096232946303270950 ) ) ;
#4745 = CARTESIAN_POINT ( 'NONE',  ( -5.859221468178921199, -2.178708437343302329, 18.97408542334169823 ) ) ;
#4746 = ADVANCED_FACE ( 'NONE', ( #6890 ), #11723, .F. ) ;
#4747 = CARTESIAN_POINT ( 'NONE',  ( 5.330189595673613390, 2.755293208590291254, 31.26382603205596311 ) ) ;
#4748 = ORIENTED_EDGE ( 'NONE', *, *, #15144, .F. ) ;
#4749 = CARTESIAN_POINT ( 'NONE',  ( -2.692693252389590786, 5.362085866495107211, 4.736173967944048435 ) ) ;
#4750 = CARTESIAN_POINT ( 'NONE',  ( -0.9739805876847252852, -5.920636045238177658, 11.76171386814421105 ) ) ;
#4752 = ORIENTED_EDGE ( 'NONE', *, *, #4839, .T. ) ;
#4751 = CARTESIAN_POINT ( 'NONE',  ( -2.500000000000000444, 1.035533905932737753, -0.7500000000000004441 ) ) ;
#4753 = CARTESIAN_POINT ( 'NONE',  ( 0.6144377077731991710, 5.969178481556046023, 23.70033966857736019 ) ) ;
#4754 = CARTESIAN_POINT ( 'NONE',  ( 0.6751155222935361078, 226.3493740387523587, 4.557952239717714349 ) ) ;
#4755 = CARTESIAN_POINT ( 'NONE',  ( -3.011385983131415145, 5.190390249166383363, 10.70047945897284158 ) ) ;
#4756 = CARTESIAN_POINT ( 'NONE',  ( 0.8561741729129451750, 2.066987299999999639, 1.200000001092474733 ) ) ;
#4757 = CARTESIAN_POINT ( 'NONE',  ( -2.773170890423259483, 226.9215440165780535, 6.244038878397168091 ) ) ;
#4758 = DIRECTION ( 'NONE',  ( 0.000000000000000000, 0.000000000000000000, -1.000000000000000000 ) ) ;
#4759 = CARTESIAN_POINT ( 'NONE',  ( -2.500000000000000444, 188.2800000002184788, 5.964466094067261359 ) ) ;
#4760 = CARTESIAN_POINT ( 'NONE',  ( -3.779082820360676109, 4.979770177899266237, 6.000049068765331839 ) ) ;
#4761 = APPLICATION_CONTEXT ( 'automotive_design' ) ;
#4762 = CARTESIAN_POINT ( 'NONE',  ( 1.080575604060385553, 227.7131986584202821, 5.411092224208442936 ) ) ;
#4763 = FACE_OUTER_BOUND ( 'NONE', #6887, .T. ) ;
#4764 = CARTESIAN_POINT ( 'NONE',  ( -2.066987299999999195, -0.8561741729129467293, -0.09999999890752520049 ) ) ;
#4765 = CARTESIAN_POINT ( 'NONE',  ( 5.558508435838253270, 2.857531096718811892, 17.99999999999998934 ) ) ;
#4766 = ORIENTED_EDGE ( 'NONE', *, *, #7650, .F. ) ;
#4767 = CARTESIAN_POINT ( 'NONE',  ( 1.461580736456473240, 187.5499999989075093, 5.538419263543526760 ) ) ;
#4768 = PRODUCT ( 'Rigid Mounting Base Clamp', 'Rigid Mounting Base Clamp', '', ( #12823 ) ) ;
#4769 = CARTESIAN_POINT ( 'NONE',  ( 1.461580736456472573, 186.5499999989075093, 8.461580736456474128 ) ) ;
#4770 = CARTESIAN_POINT ( 'NONE',  ( 5.935543223013876712, 0.8771126767605440522, 24.49999999999999289 ) ) ;
#4771 = PRODUCT_DEFINITION_FORMATION_WITH_SPECIFIED_SOURCE ( 'ANY', '', #12844, .NOT_KNOWN. ) ;
#4772 = ORIENTED_EDGE ( 'NONE', *, *, #1999, .T. ) ;
#4773 = EDGE_CURVE ( 'NONE', #9142, #11546, #13971, .T. ) ;
#4774 = B_SPLINE_CURVE_WITH_KNOTS ( 'NONE', 3,
 ( #8825, #15023, #7540, #1644, #14940, #10168, #6595, #300, #10090, #6281, #7698, #6520, #11354, #10015, #5084, #225, #11430, #1485 ),
 .UNSPECIFIED., .F., .F.,
 ( 4, 2, 2, 2, 2, 2, 2, 2, 4 ),
 ( 0.000000000000000000, 0.0003914357524127488408, 0.0007828715048254976817, 0.001174307257238246631, 0.001565743009650995363, 0.001957178762063744096, 0.002348614514476493262, 0.002740050266889241994, 0.003131486019301990727 ),
 .UNSPECIFIED. ) ;
#4775 = LINE ( 'NONE', #8524, #8579 ) ;
#4776 = CARTESIAN_POINT ( 'NONE',  ( 5.725930890718322175, -2.506952462184060426, 31.79933148907577234 ) ) ;
#4777 = DIRECTION ( 'NONE',  ( 0.000000000000000000, 0.000000000000000000, 1.000000000000000000 ) ) ;
#4778 = CARTESIAN_POINT ( 'NONE',  ( 2.066987300000000527, 186.6999999989075150, 6.143825827087054492 ) ) ;
#4779 = CARTESIAN_POINT ( 'NONE',  ( 4.195842658231382138, 4.289229542213252699, 18.50439760644211518 ) ) ;
#4780 = CARTESIAN_POINT ( 'NONE',  ( 6.176542424588115310, 0.9554180641285648923, 11.49999999999998224 ) ) ;
#4781 = DIRECTION ( 'NONE',  ( 0.000000000000000000, 0.000000000000000000, -1.000000000000000000 ) ) ;
#4782 = CARTESIAN_POINT ( 'NONE',  ( 5.931828553037973961, -0.9033193133619132897, 31.26194324003147429 ) ) ;
#4784 = CARTESIAN_POINT ( 'NONE',  ( 2.094888799673178700E-14, -6.250000000000000888, 30.00000000000000000 ) ) ;
#4783 = VECTOR ( 'NONE', #8905, 1000.000000000000000 ) ;
#4785 = CARTESIAN_POINT ( 'NONE',  ( -5.648559266344529206, 2.676764518775933244, 10.88603820591927374 ) ) ;
#4786 = CARTESIAN_POINT ( 'NONE',  ( 5.375913338529092478, 2.664979843780434621, 12.00428920362018737 ) ) ;
#4787 = VECTOR ( 'NONE', #2547, 1000.000000000000114 ) ;
#4788 = EDGE_LOOP ( 'NONE', ( #3986, #1996, #10651, #6065 ) ) ;
#4789 = ORIENTED_EDGE ( 'NONE', *, *, #13716, .T. ) ;
#4790 = VERTEX_POINT ( 'NONE', #14258 ) ;
#4791 = CARTESIAN_POINT ( 'NONE',  ( 1.789766218952369536, 227.9720476933883049, 6.158663000976825508 ) ) ;
#4792 = ORIENTED_EDGE ( 'NONE', *, *, #11, .F. ) ;
#4793 = AXIS2_PLACEMENT_3D ( 'NONE', #11299, #8617, #12411 ) ;
#4794 = AXIS2_PLACEMENT_3D ( 'NONE', #10307, #662, #1937 ) ;
#4795 = CARTESIAN_POINT ( 'NONE',  ( -1.767766952966368432, -1.767766952966369320, -2.899999997815050357 ) ) ;
#4796 = AXIS2_PLACEMENT_3D ( 'NONE', #854, #15419, #6761 ) ;
#4797 = CARTESIAN_POINT ( 'NONE',  ( -5.570722351696229424, -2.834100162822036140, 11.76190213084010416 ) ) ;
#4798 = CYLINDRICAL_SURFACE ( 'NONE', #4123, 12.50000000000000355 ) ;
#4799 = CARTESIAN_POINT ( 'NONE',  ( 2.066987300000000083, 186.0999999989075206, 6.143825827087054492 ) ) ;
#4800 = CARTESIAN_POINT ( 'NONE',  ( 2.500000000000000000, 3.061616997868383141E-16, -1.093000000021849605 ) ) ;
#4801 = CARTESIAN_POINT ( 'NONE',  ( 0.000000000000000000, 2.000000000000000000, 0.000000000000000000 ) ) ;
#4802 = CARTESIAN_POINT ( 'NONE',  ( -1.461580736456472795, 1.461580736456472795, 2.150000001092474911 ) ) ;
#4803 = CARTESIAN_POINT ( 'NONE',  ( 1.500000000000000000, -9.750000000000003553, 2.000000000000001776 ) ) ;
#4804 = CARTESIAN_POINT ( 'NONE',  ( -2.381852405317018029, 227.8773184320497478, 9.057252860304588538 ) ) ;
#4805 = LINE ( 'NONE', #14502, #2142 ) ;
#4806 = VERTEX_POINT ( 'NONE', #12412 ) ;
#4807 = AXIS2_PLACEMENT_3D ( 'NONE', #4057, #552, #1898 ) ;
#4808 = ORIENTED_EDGE ( 'NONE', *, *, #13918, .F. ) ;
#4809 = CARTESIAN_POINT ( 'NONE',  ( -5.861467994999758346E-16, 186.0999999978150754, 9.500000000000001776 ) ) ;
#4810 = ORIENTED_EDGE ( 'NONE', *, *, #11323, .T. ) ;
#4811 = ORIENTED_EDGE ( 'NONE', *, *, #8453, .T. ) ;
#4812 = DIRECTION ( 'NONE',  ( -6.123233995736766036E-17, 1.000000000000000000, 0.000000000000000000 ) ) ;
#4813 = PLANE ( 'NONE',  #4312 ) ;
#4814 = CARTESIAN_POINT ( 'NONE',  ( 0.8002720181890988771, -6.199262377003406321, 4.386062624655575171 ) ) ;
#4815 = CARTESIAN_POINT ( 'NONE',  ( -5.769755079862325609, 2.405651898698959901, 31.87305891554300530 ) ) ;
#4816 = B_SPLINE_CURVE_WITH_KNOTS ( 'NONE', 3,
 ( #4418, #6891, #8156, #9126, #10538, #4491, #9272, #13955, #3064, #11568, #14109, #6735, #663, #10385, #15236, #9345, #12118, #10849 ),
 .UNSPECIFIED., .F., .F.,
 ( 4, 2, 2, 2, 2, 2, 2, 2, 4 ),
 ( 0.000000000000000000, 0.0003914357524127467266, 0.0007828715048254934533, 0.001174307257238240126, 0.001565743009650986907, 0.001957178762063733687, 0.002348614514476480251, 0.002740050266889227249, 0.003131486019301973813 ),
 .UNSPECIFIED. ) ;
#4817 = DIRECTION ( 'NONE',  ( 0.000000000000000000, 0.000000000000000000, 1.000000000000000000 ) ) ;
#4818 =( GEOMETRIC_REPRESENTATION_CONTEXT ( 3 ) GLOBAL_UNCERTAINTY_ASSIGNED_CONTEXT ( ( #14595 ) ) GLOBAL_UNIT_ASSIGNED_CONTEXT ( ( #4204, #10330, #8995 ) ) REPRESENTATION_CONTEXT ( 'NONE', 'WORKASPACE' ) );
#4819 = CYLINDRICAL_SURFACE ( 'NONE', #8446, 2.500000000000000000 ) ;
#4820 = DIRECTION ( 'NONE',  ( -0.1736481776669306920, -0.9848077530122080203, 2.126576849575776229E-17 ) ) ;
#4821 = CARTESIAN_POINT ( 'NONE',  ( -1.530808498934191571E-16, 2.500000000000000000, -2.500000000000000000 ) ) ;
#4822 = CARTESIAN_POINT ( 'NONE',  ( -7.490007020835699691, -2.433650805992386701, 31.00000000000000000 ) ) ;
#4823 = DIRECTION ( 'NONE',  ( 0.000000000000000000, 1.000000000000000000, 0.000000000000000000 ) ) ;
#4824 = CARTESIAN_POINT ( 'NONE',  ( 2.500000000000000000, 188.6999999978150697, 7.000000000000000000 ) ) ;
#4825 = CARTESIAN_POINT ( 'NONE',  ( 2.257611286988003396, 226.6535225833466427, 5.454435118953909978 ) ) ;
#4826 = CARTESIAN_POINT ( 'NONE',  ( 4.286401442266518202, 4.198423832313208592, 31.00000000000000000 ) ) ;
#4827 = CARTESIAN_POINT ( 'NONE',  ( -1.329739968339264777, 189.0000000001359979, 4.875166081584925593 ) ) ;
#4828 = ORIENTED_EDGE ( 'NONE', *, *, #8868, .T. ) ;
#4829 = DIRECTION ( 'NONE',  ( -0.000000000000000000, 1.000000000000000000, -0.000000000000000000 ) ) ;
#4830 = CARTESIAN_POINT ( 'NONE',  ( -0.2624013748572519011, -5.995472630654522739, 10.52628559691080845 ) ) ;
#4832 = EDGE_LOOP ( 'NONE', ( #14397, #8805, #12177, #14063 ) ) ;
#4831 = CARTESIAN_POINT ( 'NONE',  ( -2.066760391300492827E-16, 189.4499999989075150, 4.933012699999999029 ) ) ;
#4833 = CARTESIAN_POINT ( 'NONE',  ( -1.354742131312345542E-14, -0.3999999999999899192, 2.455386912753366957 ) ) ;
#4834 = FACE_OUTER_BOUND ( 'NONE', #7038, .T. ) ;
#4835 = ORIENTED_EDGE ( 'NONE', *, *, #6051, .F. ) ;
#4836 = CARTESIAN_POINT ( 'NONE',  ( 2.996920846510343406, 5.485395142346868980, 23.88558052754514804 ) ) ;
#4837 = CARTESIAN_POINT ( 'NONE',  ( 3.796994071234844259E-16, -2.066987299999999639, 0.05000000109247476621 ) ) ;
#4838 = CARTESIAN_POINT ( 'NONE',  ( -2.586818446948293104, 227.7795406139177032, 8.769651989551642046 ) ) ;
#4839 = EDGE_CURVE ( 'NONE', #8675, #5801, #8468, .T. ) ;
#4840 = SURFACE_STYLE_FILL_AREA ( #3710 ) ;
#4841 = AXIS2_PLACEMENT_3D ( 'NONE', #117, #7364, #12206 ) ;
#4842 = CARTESIAN_POINT ( 'NONE',  ( -0.2637975869347698454, -6.245592211692896356, 31.97332839949191552 ) ) ;
#4843 = CARTESIAN_POINT ( 'NONE',  ( -9.825582188149883933E-17, 188.1300000002185016, 4.500000000000000000 ) ) ;
#4844 = CARTESIAN_POINT ( 'NONE',  ( 0.000000000000000000, 2.000000000000000000, -20.00000000000000000 ) ) ;
#4845 = ADVANCED_FACE ( 'NONE', ( #13388 ), #14426, .F. ) ;
#4846 = CARTESIAN_POINT ( 'NONE',  ( 0.9944270131901197241, 228.8248696211178981, 8.621661370035813121 ) ) ;
#4847 = CARTESIAN_POINT ( 'NONE',  ( -2.066987299999999639, 0.000000000000000000, -0.9499999989075252893 ) ) ;
#4848 = DIRECTION ( 'NONE',  ( 0.000000000000000000, 1.000000000000000000, 0.000000000000000000 ) ) ;
#4849 = ADVANCED_FACE ( 'NONE', ( #8400, #1140, #4894, #6005, #1511, #10848 ), #4813, .F. ) ;
#4850 = ORIENTED_EDGE ( 'NONE', *, *, #968, .F. ) ;
#4851 = CARTESIAN_POINT ( 'NONE',  ( 1.461580736456472573, 188.9499999989075150, 8.461580736456474128 ) ) ;
#4852 = CARTESIAN_POINT ( 'NONE',  ( -1.461580736456473018, 184.5499999989075093, 5.538419263543526760 ) ) ;
#4853 = LINE ( 'NONE', #6045, #14693 ) ;
#4854 = ORIENTED_EDGE ( 'NONE', *, *, #11938, .F. ) ;
#4855 = CARTESIAN_POINT ( 'NONE',  ( 0.05308131560460233739, 189.7622414119611847, 5.148053411033613358 ) ) ;
#4856 = B_SPLINE_CURVE_WITH_KNOTS ( 'NONE', 3,
 ( #8714, #9980, #2575, #7432, #1534, #2815, #3916, #1376, #12511, #3841, #6250, #1451, #5129, #266, #5050, #14831, #1611, #12588 ),
 .UNSPECIFIED., .F., .F.,
 ( 4, 2, 2, 2, 2, 2, 2, 2, 4 ),
 ( 0.003131918686235974757, 0.003523310662250265027, 0.003914702638264554863, 0.004306094614278844698, 0.004697486590293135401, 0.005088878566307425237, 0.005480270542321715940, 0.005871662518336005776, 0.006263054494350295612 ),
 .UNSPECIFIED. ) ;
#4857 = CARTESIAN_POINT ( 'NONE',  ( 5.665824935993609479, -1.978765057080921208, 5.999950536462232087 ) ) ;
#4858 = FILL_AREA_STYLE ('',( #13278 ) ) ;
#4859 = CARTESIAN_POINT ( 'NONE',  ( -3.061616997868391523E-16, 189.0000000000000000, 7.000000000000000000 ) ) ;
#4860 = CARTESIAN_POINT ( 'NONE',  ( 6.768587589771821120E-14, -6.250000000000000888, 12.49999999999998401 ) ) ;
#4861 = CARTESIAN_POINT ( 'NONE',  ( 4.286401442266437378, 4.198423832313292081, 17.99999999999998934 ) ) ;
#4862 = CARTESIAN_POINT ( 'NONE',  ( -1.530808498934191571E-16, 2.500000000000000000, -2.399999997815050801 ) ) ;
#4863 = CARTESIAN_POINT ( 'NONE',  ( 0.000000000000000000, 184.0000000000000000, 7.000000000000000000 ) ) ;
#4864 = CARTESIAN_POINT ( 'NONE',  ( 2.066987300000000527, 184.3499999989074922, 7.000000000000000000 ) ) ;
#4865 = CARTESIAN_POINT ( 'NONE',  ( 1.353717517954364224E-13, -6.250000000000000888, 18.99999999999998934 ) ) ;
#4866 = CARTESIAN_POINT ( 'NONE',  ( 5.931828553037959750, 0.9033193133620174287, 4.738056759968539922 ) ) ;
#4867 = CARTESIAN_POINT ( 'NONE',  ( -5.746837578676019298, 1.729433780394205700, 30.00004946353777413 ) ) ;
#4868 = ORIENTED_EDGE ( 'NONE', *, *, #1127, .F. ) ;
#4869 = EDGE_LOOP ( 'NONE', ( #10499, #7138 ) ) ;
#4870 = ORIENTED_EDGE ( 'NONE', *, *, #2916, .T. ) ;
#4871 = B_SPLINE_CURVE_WITH_KNOTS ( 'NONE', 3,
 ( #3702, #7373, #4830, #1311, #2187, #10789, #9840, #1002, #6109, #9686, #4750, #14525, #14356, #8331, #13169, #3625, #2432, #1238 ),
 .UNSPECIFIED., .F., .F.,
 ( 4, 2, 2, 2, 2, 2, 2, 2, 4 ),
 ( 0.003131923598876997904, 0.003523316383094314812, 0.003914709167311631287, 0.004306101951528948195, 0.004697494735746265103, 0.005088887519963581144, 0.005480280304180898052, 0.005871673088398214960, 0.006263065872615531868 ),
 .UNSPECIFIED. ) ;
#4872 = DIRECTION ( 'NONE',  ( -1.000000000000000000, 0.000000000000000000, 0.000000000000000000 ) ) ;
#4873 = VERTEX_POINT ( 'NONE', #13312 ) ;
#4874 = AXIS2_PLACEMENT_3D ( 'NONE', #7605, #2835, #2988 ) ;
#4875 = CARTESIAN_POINT ( 'NONE',  ( 1.461580736456472573, 1.461580736456472795, 0.9500000010924747329 ) ) ;
#4876 = CARTESIAN_POINT ( 'NONE',  ( 0.000000000000000000, 22.00000000000000000, 0.000000000000000000 ) ) ;
#4877 = DIRECTION ( 'NONE',  ( 0.000000000000000000, 0.000000000000000000, 1.000000000000000000 ) ) ;
#4878 = CARTESIAN_POINT ( 'NONE',  ( 2.066987300000000083, 186.0499999989075093, 7.000000000000000000 ) ) ;
#4879 = CARTESIAN_POINT ( 'NONE',  ( -2.500000000000000444, 1.035533905932737753, -2.343000000021849605 ) ) ;
#4880 = DIRECTION ( 'NONE',  ( 0.000000000000000000, 2.775557561562887900E-16, -1.000000000000000000 ) ) ;
#4881 = CARTESIAN_POINT ( 'NONE',  ( 4.195842658231482503, 4.289229542213157664, 5.504397606442132052 ) ) ;
#4882 = CARTESIAN_POINT ( 'NONE',  ( 2.066987300000000083, -0.8561741729129449530, -1.599999998907525534 ) ) ;
#4883 = ADVANCED_FACE ( 'NONE', ( #7281 ), #6088, .F. ) ;
#4884 = CARTESIAN_POINT ( 'NONE',  ( 4.153663429050823197, -4.670992970568335068, 30.20066851092421700 ) ) ;
#4885 = CARTESIAN_POINT ( 'NONE',  ( -1.979540121751099724, 226.5646310999674427, 5.192482286045976281 ) ) ;
#4886 = CARTESIAN_POINT ( 'NONE',  ( 6.021135683317679899, 1.680226122398283950, 5.973772828752684561 ) ) ;
#4887 = ORIENTED_EDGE ( 'NONE', *, *, #8312, .F. ) ;
#4888 = AXIS2_PLACEMENT_3D ( 'NONE', #4339, #3144, #7996 ) ;
#4889 = MANIFOLD_SOLID_BREP ( 'Extrude-Thin1', #2413 ) ;
#4890 = EDGE_LOOP ( 'NONE', ( #12376, #935 ) ) ;
#4891 = ORIENTED_EDGE ( 'NONE', *, *, #2586, .T. ) ;
#4892 = ORIENTED_EDGE ( 'NONE', *, *, #4101, .T. ) ;
#4893 = CARTESIAN_POINT ( 'NONE',  ( 0.9740012993920327267, 6.173846968979637140, 31.26164920628441024 ) ) ;
#4894 = FACE_BOUND ( 'NONE', #4727, .T. ) ;
#4895 = CARTESIAN_POINT ( 'NONE',  ( 0.5043776560897352823, -6.230795654995838539, 5.873374762960125395 ) ) ;
#4896 = CARTESIAN_POINT ( 'NONE',  ( 0.000000000000000000, 0.000000000000000000, 0.000000000000000000 ) ) ;
#4897 = B_SPLINE_CURVE_WITH_KNOTS ( 'NONE', 3,
 ( #7971, #3270, #5438, #1994, #7814, #13851, #6712, #10285, #7895, #11624, #6868, #10208, #12812, #10440, #4233, #9101, #9026, #10360 ),
 .UNSPECIFIED., .F., .F.,
 ( 4, 2, 2, 2, 2, 2, 2, 2, 4 ),
 ( 0.003131486019301974247, 0.003522824630466683121, 0.003914163241631391996, 0.004305501852796101737, 0.004696840463960810612, 0.005088179075125519486, 0.005479517686290229228, 0.005870856297454939837, 0.006262194908619649579 ),
 .UNSPECIFIED. ) ;
#4898 = DIRECTION ( 'NONE',  ( -0.000000000000000000, 1.000000000000000000, -0.000000000000000000 ) ) ;
#4899 = CARTESIAN_POINT ( 'NONE',  ( -3.011385983131359190, -5.190390249166418002, 12.29952054102714598 ) ) ;
#4900 = AXIS2_PLACEMENT_3D ( 'NONE', #3938, #14697, #5073 ) ;
#4901 = CARTESIAN_POINT ( 'NONE',  ( -5.903061651806636334, 2.057626436184698537, 5.999917418102894473 ) ) ;
#4902 = CARTESIAN_POINT ( 'NONE',  ( 2.817313151351065859, -5.579000502529494199, 17.99999999999998934 ) ) ;
#4903 = DIRECTION ( 'NONE',  ( 0.000000000000000000, 0.000000000000000000, -1.000000000000000000 ) ) ;
#4904 = DIRECTION ( 'NONE',  ( 1.000000000000000000, 0.000000000000000000, 1.047444401652940007E-14 ) ) ;
#4905 = CARTESIAN_POINT ( 'NONE',  ( 2.500000000000000444, 187.1499999978150868, 5.964466094067262247 ) ) ;
#4906 = CARTESIAN_POINT ( 'NONE',  ( -0.1001789588503840533, 226.3251931448050698, 4.486704830075608719 ) ) ;
#4907 = CARTESIAN_POINT ( 'NONE',  ( 5.409274167810647072, 2.597759609440661421, 10.88480617551147667 ) ) ;
#4908 = CARTESIAN_POINT ( 'NONE',  ( -2.488587570294162443, 189.3796024022271922, 5.337940027815102795 ) ) ;
#4909 = AXIS2_PLACEMENT_3D ( 'NONE', #5114, #1437, #13375 ) ;
#4910 = ORIENTED_EDGE ( 'NONE', *, *, #8830, .F. ) ;
#4911 = CARTESIAN_POINT ( 'NONE',  ( 2.000000000000001776, 5.005650134388747156E-16, -1.500000000000000000 ) ) ;
#4912 = CARTESIAN_POINT ( 'NONE',  ( 0.2622916576877225014, -5.995491482261829042, 12.47384942646812078 ) ) ;
#4913 = DIRECTION ( 'NONE',  ( 0.000000000000000000, 0.000000000000000000, 1.000000000000000000 ) ) ;
#4914 = CARTESIAN_POINT ( 'NONE',  ( 4.435347140101058905, -4.403429997944484420, 31.00000000000000000 ) ) ;
#4915 = CARTESIAN_POINT ( 'NONE',  ( 0.3831815474498145857, 226.3309662840062515, 4.503685043354857420 ) ) ;
#4916 = CARTESIAN_POINT ( 'NONE',  ( -4.006441409774768481, 4.467329318258185467, 10.70111757752057002 ) ) ;
#4917 = B_SPLINE_CURVE_WITH_KNOTS ( 'NONE', 1,
 ( #12435, #9828 ),
 .UNSPECIFIED., .F., .F.,
 ( 2, 2 ),
 ( 0.000000000000000000, 1.000000000000000000 ),
 .UNSPECIFIED. ) ;
#4918 = CARTESIAN_POINT ( 'NONE',  ( 0.8561741729129463963, -2.066987299999999195, 0.9000000010924746885 ) ) ;
#4919 = CARTESIAN_POINT ( 'NONE',  ( 2.031800923730693940E-13, -6.250000000000000888, 23.49999999999999289 ) ) ;
#4920 = AXIS2_PLACEMENT_3D ( 'NONE', #12576, #4224, #10124 ) ;
#4921 = CARTESIAN_POINT ( 'NONE',  ( -0.1306070469493167963, -6.250000000000002665, 30.00000000000000000 ) ) ;
#4922 = CARTESIAN_POINT ( 'NONE',  ( 2.500000000000000444, 187.1300000002185016, 7.000000000000000000 ) ) ;
#4923 = FACE_BOUND ( 'NONE', #2983, .T. ) ;
#4924 = CARTESIAN_POINT ( 'NONE',  ( 1.965304387191771029, 228.1545866171788930, 6.685845824222668377 ) ) ;
#4925 = CARTESIAN_POINT ( 'NONE',  ( -1.265664690411614835E-16, 2.066987299999999639, 2.050000001092474822 ) ) ;
#4926 = CARTESIAN_POINT ( 'NONE',  ( 5.558508435838323436, -2.857531096718671559, 24.63237410716305931 ) ) ;
#4927 = ORIENTED_EDGE ( 'NONE', *, *, #15329, .F. ) ;
#4928 = DIRECTION ( 'NONE',  ( -0.000000000000000000, 1.000000000000000000, -0.000000000000000000 ) ) ;
#4929 = CARTESIAN_POINT ( 'NONE',  ( 1.461580736456473462, 185.1499999989075320, 5.538419263543526760 ) ) ;
#4930 = CARTESIAN_POINT ( 'NONE',  ( -7.490007020835699691, -2.433650805992386701, 31.00000000000000000 ) ) ;
#4932 = ORIENTED_EDGE ( 'NONE', *, *, #12404, .F. ) ;
#4931 = CARTESIAN_POINT ( 'NONE',  ( 3.780072143464197065, 4.979057943639763728, 29.99991780678444186 ) ) ;
#4933 = AXIS2_PLACEMENT_3D ( 'NONE', #81, #12012, #12248 ) ;
#4934 = ADVANCED_FACE ( 'NONE', ( #9751 ), #1744, .F. ) ;
#4935 = FACE_OUTER_BOUND ( 'NONE', #14312, .T. ) ;
#4936 = CARTESIAN_POINT ( 'NONE',  ( 5.531796221294873028, -2.326749136277222796, 5.873784308702619583 ) ) ;
#4937 = DIRECTION ( 'NONE',  ( -6.123233995736766036E-17, 1.000000000000000000, 0.000000000000000000 ) ) ;
#4938 = CARTESIAN_POINT ( 'NONE',  ( 5.999999999999999112, 186.5669965222008670, 9.317226423031115701 ) ) ;
#4939 = CARTESIAN_POINT ( 'NONE',  ( -0.7988860301921629770, -6.199427171881343845, 10.88455580536193601 ) ) ;
#4940 = CARTESIAN_POINT ( 'NONE',  ( 3.312524433819871827, -5.004191858253940417, 30.02591947216899371 ) ) ;
#4941 = CARTESIAN_POINT ( 'NONE',  ( 0.1189749320691910750, 189.0435645138963139, 10.18765630333474626 ) ) ;
#4942 = CARTESIAN_POINT ( 'NONE',  ( 7.799024015210631156, -1.482594289697088730, 5.000000000000004441 ) ) ;
#4943 = MANIFOLD_SOLID_BREP ( 'AdvancedHole3', #3684 ) ;
#4944 = CARTESIAN_POINT ( 'NONE',  ( 5.746619684944286099, -1.730157667110801212, 32.00004932073311892 ) ) ;
#4945 = CARTESIAN_POINT ( 'NONE',  ( -5.666074146198012862, 1.978051345703121244, 10.49995067926686332 ) ) ;
#4946 = CARTESIAN_POINT ( 'NONE',  ( 5.903347812666339678, 1.076697810262650323, 4.386022610569179747 ) ) ;
#4947 = CARTESIAN_POINT ( 'NONE',  ( 2.668367453516445664, 5.373994336898223700, 24.36938304467862082 ) ) ;
#4948 = EDGE_CURVE ( 'NONE', #15526, #5163, #11221, .T. ) ;
#4949 = ORIENTED_EDGE ( 'NONE', *, *, #13803, .T. ) ;
#4950 = VERTEX_POINT ( 'NONE', #1822 ) ;
#4951 = AXIS2_PLACEMENT_3D ( 'NONE', #10470, #15324, #4424 ) ;
#4952 = ADVANCED_FACE ( 'NONE', ( #9009 ), #3973, .T. ) ;
#4953 = ORIENTED_EDGE ( 'NONE', *, *, #9926, .T. ) ;
#4954 = CARTESIAN_POINT ( 'NONE',  ( -4.286401442266607020, 4.198423832313117110, 31.00000000000000000 ) ) ;
#4955 = ORIENTED_EDGE ( 'NONE', *, *, #5899, .F. ) ;
#4956 = CARTESIAN_POINT ( 'NONE',  ( 0.8561741729129463963, -2.066987299999999195, -0.8999999989075251339 ) ) ;
#4957 = EDGE_CURVE ( 'NONE', #7973, #12251, #4093, .T. ) ;
#4958 = CARTESIAN_POINT ( 'NONE',  ( -6.155867707731093930, -1.081837891425983189, 12.00436969680152899 ) ) ;
#4959 = CARTESIAN_POINT ( 'NONE',  ( 0.8561741729129458411, 187.4999999989075548, 9.066987299999999195 ) ) ;
#4960 = CARTESIAN_POINT ( 'NONE',  ( 1.767766952966368654, 1.767766952966369098, 1.399999999999999911 ) ) ;
#4961 = AXIS2_PLACEMENT_3D ( 'NONE', #8228, #15308, #13063 ) ;
#4962 = CARTESIAN_POINT ( 'NONE',  ( -5.409007216690699948, 2.598315788643695612, 31.61442521571937547 ) ) ;
#4963 = CARTESIAN_POINT ( 'NONE',  ( 4.286401442266577710, -4.198423832313146420, 31.00000000000000000 ) ) ;
#4964 = CARTESIAN_POINT ( 'NONE',  ( 2.066987299999999639, 0.8561741729129456191, -1.499999998907525445 ) ) ;
#4965 = EDGE_CURVE ( 'NONE', #1061, #6866, #9367, .T. ) ;
#4966 = CARTESIAN_POINT ( 'NONE',  ( 2.996417732210637563, -5.485687819086870753, 30.38603820591928084 ) ) ;
#4967 = CARTESIAN_POINT ( 'NONE',  ( -2.990426535912302786, 227.3682058476787233, 7.559219386994686651 ) ) ;
#4968 = CARTESIAN_POINT ( 'NONE',  ( 5.985119669071089277, 1.805077827356658116, 5.999917418102894473 ) ) ;
#4969 = ORIENTED_EDGE ( 'NONE', *, *, #3477, .T. ) ;
#4970 = ORIENTED_EDGE ( 'NONE', *, *, #13089, .F. ) ;
#4971 = EDGE_LOOP ( 'NONE', ( #3659, #4338, #6283, #11005 ) ) ;
#4972 = VERTEX_POINT ( 'NONE', #5346 ) ;
#4973 = CARTESIAN_POINT ( 'NONE',  ( 2.388242816781450006, 189.0000000000000000, 6.240296789758633444 ) ) ;
#4974 = CARTESIAN_POINT ( 'NONE',  ( 0.6151877315909851651, -6.220340188096018075, 5.799066734696703307 ) ) ;
#4975 = EDGE_CURVE ( 'NONE', #4214, #12581, #3269, .T. ) ;
#4976 = CARTESIAN_POINT ( 'NONE',  ( 4.005785023174466275, -4.467917056767390704, 12.29952054102713532 ) ) ;
#4977 = CARTESIAN_POINT ( 'NONE',  ( 4.416779112813571828, -4.422345839825880809, 24.23774718278286855 ) ) ;
#4978 = DIRECTION ( 'NONE',  ( 0.000000000000000000, 1.000000000000000000, 0.000000000000000000 ) ) ;
#4979 = CARTESIAN_POINT ( 'NONE',  ( -3.781065399486036149, 4.978303713186424062, 10.50008258189709132 ) ) ;
#4980 = CARTESIAN_POINT ( 'NONE',  ( -1.035533905932737753, 2.500000000000000444, -2.450000000000000178 ) ) ;
#4981 = DIRECTION ( 'NONE',  ( -1.000000000000000000, 0.000000000000000000, 0.000000000000000000 ) ) ;
#4982 = CARTESIAN_POINT ( 'NONE',  ( 6.805491029613696752E-14, 106.0000000000000142, -9.750000000000003553 ) ) ;
#4983 = CARTESIAN_POINT ( 'NONE',  ( -1.767766952966369320, 187.3999999978150584, 5.232233047033630235 ) ) ;
#4984 = CARTESIAN_POINT ( 'NONE',  ( 2.923059718105053051, 227.5089953743221258, 7.973592892444406388 ) ) ;
#4985 = DIRECTION ( 'NONE',  ( 0.000000000000000000, 0.000000000000000000, 1.000000000000000000 ) ) ;
#4986 = CARTESIAN_POINT ( 'NONE',  ( -1.135771517436445111, 189.0000000004517631, 9.231728281961022020 ) ) ;
#4987 = ORIENTED_EDGE ( 'NONE', *, *, #8342, .T. ) ;
#4988 = CARTESIAN_POINT ( 'NONE',  ( -5.931734679891446760, 0.9039278060244116952, 11.76382603205595956 ) ) ;
#4989 = FACE_OUTER_BOUND ( 'NONE', #10106, .T. ) ;
#4990 = CARTESIAN_POINT ( 'NONE',  ( 2.500000000000000000, 188.0000000000000000, 7.000000000000000000 ) ) ;
#4991 = CARTESIAN_POINT ( 'NONE',  ( 4.344265632482167128, -4.493596842504882005, 31.50425949503009448 ) ) ;
#4992 = CARTESIAN_POINT ( 'NONE',  ( 1.815011834558647452, 226.5209060679430308, 5.063596875652942586 ) ) ;
#4993 = ADVANCED_FACE ( 'NONE', ( #554 ), #397, .F. ) ;
#4994 = CARTESIAN_POINT ( 'NONE',  ( 7.180990026460783326, -3.384707322287269893, 17.99999999999998934 ) ) ;
#4995 = CARTESIAN_POINT ( 'NONE',  ( -1.461580736456472795, 1.461580736456472795, 0.5500000010924748217 ) ) ;
#4996 = CARTESIAN_POINT ( 'NONE',  ( -3.159082487394956118, 5.393634094348230157, 23.70045537531157365 ) ) ;
#4997 = CARTESIAN_POINT ( 'NONE',  ( -5.558508435838198203, 2.857531096718914032, 11.63060690723495760 ) ) ;
#4998 = CARTESIAN_POINT ( 'NONE',  ( 1.767766952966368432, 187.8300000002184902, 8.767766952966368876 ) ) ;
#4999 = FACE_BOUND ( 'NONE', #13681, .T. ) ;
#5000 = CARTESIAN_POINT ( 'NONE',  ( 1.558909820229182230, 228.6656996696739554, 8.161969471806774123 ) ) ;
#5001 = CARTESIAN_POINT ( 'NONE',  ( -2.066987299999999195, -0.8561741729129467293, -2.499999998907525001 ) ) ;
#5002 = FACE_OUTER_BOUND ( 'NONE', #11159, .T. ) ;
#5003 = ORIENTED_EDGE ( 'NONE', *, *, #8249, .T. ) ;
#5004 = CARTESIAN_POINT ( 'NONE',  ( -0.8561741729129455081, 2.066987299999999639, 1.900000001092474911 ) ) ;
#5005 = CARTESIAN_POINT ( 'NONE',  ( -0.8561741729129470624, 186.3999999989075320, 9.066987300000000971 ) ) ;
#5006 = CARTESIAN_POINT ( 'NONE',  ( -2.997753866155795421, -5.484939622623858924, 12.11560192892921251 ) ) ;
#5008 = VERTEX_POINT ( 'NONE', #10191 ) ;
#5007 = CARTESIAN_POINT ( 'NONE',  ( -0.8561741729129467293, 185.7999999989075093, 9.066987299999999195 ) ) ;
#5009 = CYLINDRICAL_SURFACE ( 'NONE', #244, 5.000000000000000000 ) ;
#5010 = CARTESIAN_POINT ( 'NONE',  ( 1.547212085679566465E-16, 22.00000000000000000, -11.25000000000000355 ) ) ;
#5011 = DIRECTION ( 'NONE',  ( 0.5877852522924802425, -0.8090169943749422332, 0.000000000000000000 ) ) ;
#5012 = VECTOR ( 'NONE', #2121, 1000.000000000000114 ) ;
#5013 = CARTESIAN_POINT ( 'NONE',  ( 5.999999999999999112, 215.0542865858234336, 7.296348638370669271 ) ) ;
#5014 = CARTESIAN_POINT ( 'NONE',  ( -2.434916734102785085, 189.0000000000000000, 7.580643601937843812 ) ) ;
#5015 = CARTESIAN_POINT ( 'NONE',  ( 3.633127580202159201, 4.776802569231145768, 16.99992038825522656 ) ) ;
#5016 = LINE ( 'NONE', #152, #9044 ) ;
#5017 = CARTESIAN_POINT ( 'NONE',  ( -0.8738118504725461699, -5.936246475285035018, 31.50357242174242600 ) ) ;
#5018 = CARTESIAN_POINT ( 'NONE',  ( 5.915699123067170717, -1.003533581835479582, 31.50389795015983552 ) ) ;
#5019 = CARTESIAN_POINT ( 'NONE',  ( -3.567258970015989128, 5.133675764669665575, 29.99991780678443121 ) ) ;
#5020 = CARTESIAN_POINT ( 'NONE',  ( -5.931817299736859894, 0.9033986943601567399, 30.73770962164068621 ) ) ;
#5021 = EDGE_CURVE ( 'NONE', #2326, #10913, #15043, .T. ) ;
#5022 = ORIENTED_EDGE ( 'NONE', *, *, #594, .T. ) ;
#5023 = EDGE_LOOP ( 'NONE', ( #1993, #9158 ) ) ;
#5024 = AXIS2_PLACEMENT_3D ( 'NONE', #13036, #6933, #10737 ) ;
#5025 = EDGE_LOOP ( 'NONE', ( #13522, #5572 ) ) ;
#5026 = CARTESIAN_POINT ( 'NONE',  ( -5.317509234263835260, -2.779225709351231366, 24.63064961348855775 ) ) ;
#5027 = ORIENTED_EDGE ( 'NONE', *, *, #2740, .F. ) ;
#5028 = CARTESIAN_POINT ( 'NONE',  ( 2.066987299999999639, 0.8561741729129456191, -0.6999999989075255113 ) ) ;
#5029 = FACE_BOUND ( 'NONE', #7879, .T. ) ;
#5030 = CARTESIAN_POINT ( 'NONE',  ( -1.461580736456473906, 188.7499999989075263, 8.461580736456474128 ) ) ;
#5031 = CYLINDRICAL_SURFACE ( 'NONE', #15305, 1.000000000000000666 ) ;
#5032 = CARTESIAN_POINT ( 'NONE',  ( -9.750000000000003553, 182.0000000000000000, 1.499999999999965583 ) ) ;
#5033 = CARTESIAN_POINT ( 'NONE',  ( -2.500000000000000000, 0.000000000000000000, -2.293000000021850227 ) ) ;
#5034 = VECTOR ( 'NONE', #4125, 1000.000000000000000 ) ;
#5035 = CARTESIAN_POINT ( 'NONE',  ( -5.317509234263962270, 2.779225709350992890, 31.13061695532139339 ) ) ;
#5036 = ADVANCED_FACE ( 'NONE', ( #8117 ), #1978, .F. ) ;
#5037 = CONTEXT_DEPENDENT_SHAPE_REPRESENTATION ( #10863, #2477 ) ;
#5038 = CARTESIAN_POINT ( 'NONE',  ( 2.668367453516629517, 5.373994336898132218, 5.000000000000004441 ) ) ;
#5039 = CARTESIAN_POINT ( 'NONE',  ( -2.066987299999999195, -0.8561741729129466183, -1.099999998907525089 ) ) ;
#5040 = FACE_OUTER_BOUND ( 'NONE', #2809, .T. ) ;
#5041 = CARTESIAN_POINT ( 'NONE',  ( -2.809592974547592714, 227.6294044507834542, 8.327915135215583575 ) ) ;
#5042 = EDGE_CURVE ( 'NONE', #5984, #9644, #14323, .T. ) ;
#5043 = EDGE_LOOP ( 'NONE', ( #14358, #3210 ) ) ;
#5044 = ORIENTED_EDGE ( 'NONE', *, *, #10805, .T. ) ;
#5045 = ADVANCED_FACE ( 'NONE', ( #10574 ), #2131, .F. ) ;
#5046 = ORIENTED_EDGE ( 'NONE', *, *, #3851, .F. ) ;
#5047 = CARTESIAN_POINT ( 'NONE',  ( 0.9737778612006920964, 5.920671847850494274, 17.73736375884652716 ) ) ;
#5048 = CARTESIAN_POINT ( 'NONE',  ( 2.841163418881393454, 5.567120626447931819, 4.737630265561252330 ) ) ;
#5049 = CARTESIAN_POINT ( 'NONE',  ( -6.081509788407712058, -1.446521464462831918, 17.12618035954928075 ) ) ;
#5050 = CARTESIAN_POINT ( 'NONE',  ( -2.782769401326246062, -5.315896561274812804, 18.50428920362019269 ) ) ;
#5051 = CARTESIAN_POINT ( 'NONE',  ( 1.734723475976807094E-15, -0.001000000000000132727, 13.50000000000000000 ) ) ;
#5052 = CARTESIAN_POINT ( 'NONE',  ( -0.5042675786777256475, -6.230788509548854215, 25.37331068310447080 ) ) ;
#5053 = CARTESIAN_POINT ( 'NONE',  ( -3.883588957979273726, 4.898466244118916180, 10.52622717124729412 ) ) ;
#5054 = CARTESIAN_POINT ( 'NONE',  ( -2.817313151351311884, 5.579000502529370742, 17.99999999999998934 ) ) ;
#5055 = CARTESIAN_POINT ( 'NONE',  ( 0.000000000000000000, 142.0000000000000000, 0.000000000000000000 ) ) ;
#5056 = CIRCLE ( 'NONE', #6070, 7.000000000000000000 ) ;
#5057 = CARTESIAN_POINT ( 'NONE',  ( -1.035533905932737975, 186.6199999975965511, 4.500000000000000888 ) ) ;
#5058 = CARTESIAN_POINT ( 'NONE',  ( 0.6422548253168780530, 227.6434438162357878, 5.209636261422765813 ) ) ;
#5059 = AXIS2_PLACEMENT_3D ( 'NONE', #5117, #11311, #6477 ) ;
#5060 = CARTESIAN_POINT ( 'NONE',  ( 2.550395957922052759, 226.7806086135062458, 5.828878098564913124 ) ) ;
#5061 = CARTESIAN_POINT ( 'NONE',  ( -2.662230360837048337, 189.2020403679304366, 8.562491460291731471 ) ) ;
#5062 = ORIENTED_EDGE ( 'NONE', *, *, #10429, .F. ) ;
#5063 = DIRECTION ( 'NONE',  ( 0.9510565162951499785, 0.3090169943749582204, 0.000000000000000000 ) ) ;
#5064 = APPLICATION_CONTEXT ( 'automotive_design' ) ;
#5065 = CARTESIAN_POINT ( 'NONE',  ( 3.779681992289830372, -4.979315417303873836, 10.50004921015705150 ) ) ;
#5066 = AXIS2_PLACEMENT_3D ( 'NONE', #7954, #9008, #15042 ) ;
#5067 = CARTESIAN_POINT ( 'NONE',  ( -3.011385983131546595, 5.190390249166308756, 23.70047945897283270 ) ) ;
#5068 = FACE_OUTER_BOUND ( 'NONE', #10463, .T. ) ;
#5069 = CARTESIAN_POINT ( 'NONE',  ( 2.228329245637216793, 227.9362088727311857, 9.230470988095557772 ) ) ;
#5070 = CARTESIAN_POINT ( 'NONE',  ( 3.253823204784968226, 5.337590213880594625, 23.62694108445698760 ) ) ;
#5071 = EDGE_CURVE ( 'NONE', #12251, #10913, #2979, .T. ) ;
#5072 = CARTESIAN_POINT ( 'NONE',  ( 1.035533905932737531, 2.500000000000000444, 2.250000000000000444 ) ) ;
#5073 = DIRECTION ( 'NONE',  ( -0.3090169943749446202, -0.9510565162951544194, 0.000000000000000000 ) ) ;
#5074 = FILL_AREA_STYLE_COLOUR ( '', #9398 ) ;
#5075 = LINE ( 'NONE', #3787, #612 ) ;
#5076 = CARTESIAN_POINT ( 'NONE',  ( -6.369687763352338550E-16, 186.9300000002185129, 9.500000000000001776 ) ) ;
#5077 = CARTESIAN_POINT ( 'NONE',  ( 1.862843374206504254, 228.4903663355887318, 7.655596802610238782 ) ) ;
#5078 = DIRECTION ( 'NONE',  ( 0.000000000000000000, 0.000000000000000000, -1.000000000000000000 ) ) ;
#5079 = EDGE_CURVE ( 'NONE', #9324, #6928, #14723, .T. ) ;
#5080 = CARTESIAN_POINT ( 'NONE',  ( -3.779082820360647244, -4.979770177899287553, 10.49995093123465395 ) ) ;
#5081 = AXIS2_PLACEMENT_3D ( 'NONE', #2908, #280, #5144 ) ;
#5082 = CARTESIAN_POINT ( 'NONE',  ( 6.123233995736766282E-16, -6.250000000000000888, 6.000000000000004441 ) ) ;
#5083 = CARTESIAN_POINT ( 'NONE',  ( 1.461580736456472573, 188.1499999989075036, 8.461580736456474128 ) ) ;
#5084 = CARTESIAN_POINT ( 'NONE',  ( 6.155912734541153952, -1.081577393120774166, 18.50389213124969956 ) ) ;
#5086 = EDGE_LOOP ( 'NONE', ( #1056, #5326, #9418, #11292 ) ) ;
#5085 = CARTESIAN_POINT ( 'NONE',  ( -1.084202172485504434E-15, -3.464101615137755275, -2.500000000000000000 ) ) ;
#5087 = CARTESIAN_POINT ( 'NONE',  ( -4.005361199355111701, -4.468319061418669413, 23.69977782616122397 ) ) ;
#5088 = MECHANICAL_DESIGN_GEOMETRIC_PRESENTATION_REPRESENTATION (  '', ( #3804 ), #10931 ) ;
#5089 = LINE ( 'NONE', #10174, #11620 ) ;
#5090 = CARTESIAN_POINT ( 'NONE',  ( 2.735911510694367108E-17, 7.147123651097129995E-16, -2.575022672948154234 ) ) ;
#5091 = B_SPLINE_CURVE_WITH_KNOTS ( 'NONE', 3,
 ( #14011, #13931, #11703, #11543, #11394, #643, #5514, #4396, #9250, #14084, #8052, #12890, #5670, #1334, #10671, #11848, #13434, #10968 ),
 .UNSPECIFIED., .F., .F.,
 ( 4, 2, 2, 2, 2, 2, 2, 2, 4 ),
 ( 0.003131918686235979962, 0.003523310662250269364, 0.003914702638264559199, 0.004306094614278848168, 0.004697486590293138004, 0.005088878566307427839, 0.005480270542321717675, 0.005871662518336009245, 0.006263054494350299081 ),
 .UNSPECIFIED. ) ;
#5092 = CARTESIAN_POINT ( 'NONE',  ( 0.07962197837297851910, 190.0874091994478761, 4.202769589527710181 ) ) ;
#5093 = CARTESIAN_POINT ( 'NONE',  ( -0.6144300524833031796, -6.220417338033058741, 10.70033372175932662 ) ) ;
#5094 = CARTESIAN_POINT ( 'NONE',  ( 1.767766952966369320, -1.767766952966368654, 0.3999999999999997446 ) ) ;
#5095 = CARTESIAN_POINT ( 'NONE',  ( 2.500000000000000444, -1.035533905932737309, -2.649999997815050357 ) ) ;
#5096 = CARTESIAN_POINT ( 'NONE',  ( 2.094888798833199608E-14, -6.000000000000000888, 30.00000000000000000 ) ) ;
#5097 = CARTESIAN_POINT ( 'NONE',  ( 4.141923667210722471, -4.342011609040392628, 5.615617326986045654 ) ) ;
#5098 = CARTESIAN_POINT ( 'NONE',  ( -1.000082492230581765, -6.169467968613729703, 18.13152538105390832 ) ) ;
#5099 = CARTESIAN_POINT ( 'NONE',  ( -5.931817299736839466, -0.9033986943602941855, 11.76229037835932800 ) ) ;
#5100 = LINE ( 'NONE', #7407, #14564 ) ;
#5101 = EDGE_LOOP ( 'NONE', ( #2144, #5592, #10151, #14399 ) ) ;
#5102 = CARTESIAN_POINT ( 'NONE',  ( 2.066987300000000083, 187.6499999989075320, 7.000000000000000000 ) ) ;
#5103 = ORIENTED_EDGE ( 'NONE', *, *, #6150, .F. ) ;
#5104 = DIRECTION ( 'NONE',  ( 0.000000000000000000, 0.000000000000000000, 1.000000000000000000 ) ) ;
#5105 = EDGE_LOOP ( 'NONE', ( #879, #10287, #15216, #2305 ) ) ;
#5106 = DIRECTION ( 'NONE',  ( 0.000000000000000000, 0.000000000000000000, -1.000000000000000000 ) ) ;
#5107 = ORIENTED_EDGE ( 'NONE', *, *, #10989, .F. ) ;
#5108 = CARTESIAN_POINT ( 'NONE',  ( -1.265664690411614835E-16, 2.066987299999999639, -1.349999998907525534 ) ) ;
#5109 = CARTESIAN_POINT ( 'NONE',  ( 5.726049995854488373, 2.506679546901831035, 18.79954462468841925 ) ) ;
#5110 = CARTESIAN_POINT ( 'NONE',  ( -2.246716568442826745, 227.9318189537954993, 9.217556643805876249 ) ) ;
#5111 = CYLINDRICAL_SURFACE ( 'NONE', #13257, 2.500000000000000000 ) ;
#5112 = CARTESIAN_POINT ( 'NONE',  ( -2.500000000000000000, -0.9567085809127248153, 2.546193976625564126 ) ) ;
#5113 = B_SPLINE_CURVE_WITH_KNOTS ( 'NONE', 3,
 ( #8876, #12589, #14908, #1922, #2816, #3999, #10214, #6564, #576, #647, #7665, #1767, #11472, #12513, #420, #13937, #2893, #10139 ),
 .UNSPECIFIED., .F., .F.,
 ( 4, 2, 2, 2, 2, 2, 2, 2, 4 ),
 ( 0.000000000000000000, 0.0003914362731607440218, 0.0007828725463214880435, 0.001174308819482232065, 0.001565745092642976087, 0.001957181365803720326, 0.002348617638964464131, 0.002740053912125207936, 0.003131490185285952174 ),
 .UNSPECIFIED. ) ;
#5114 = CARTESIAN_POINT ( 'NONE',  ( -13.50000000000000000, -0.001000000000000132727, 2.479909768273400161E-15 ) ) ;
#5115 = CARTESIAN_POINT ( 'NONE',  ( 4.142173849413761211, 4.341773579105392855, 5.615193824488510010 ) ) ;
#5116 = CARTESIAN_POINT ( 'NONE',  ( -2.066987299999999639, 0.000000000000000000, 0.6500000010924747995 ) ) ;
#5117 = CARTESIAN_POINT ( 'NONE',  ( -7.490007020835664164, -2.433650805992495503, 17.99999999999998934 ) ) ;
#5118 = CARTESIAN_POINT ( 'NONE',  ( -2.623350778723538834, 226.8212935938476278, 5.948734516926445615 ) ) ;
#5119 = ORIENTED_EDGE ( 'NONE', *, *, #9140, .F. ) ;
#5120 = ORIENTED_EDGE ( 'NONE', *, *, #14369, .F. ) ;
#5121 = VERTEX_POINT ( 'NONE', #13033 ) ;
#5122 = VECTOR ( 'NONE', #1160, 1000.000000000000000 ) ;
#5123 = CARTESIAN_POINT ( 'NONE',  ( 0.2624013748574551275, 5.995472630654512969, 17.02628559691081733 ) ) ;
#5124 = CARTESIAN_POINT ( 'NONE',  ( 1.458225638478870767, 188.9999999999999716, 4.936243315740555637 ) ) ;
#5125 = ADVANCED_FACE ( 'NONE', ( #9384 ), #11606, .F. ) ;
#5126 = ORIENTED_EDGE ( 'NONE', *, *, #5848, .F. ) ;
#5127 = CARTESIAN_POINT ( 'NONE',  ( 0.5042675786779255986, 6.230788509548840004, 5.873310683104476126 ) ) ;
#5128 = ADVANCED_FACE ( 'NONE', ( #7003 ), #8276, .T. ) ;
#5129 = CARTESIAN_POINT ( 'NONE',  ( -3.011385983131411592, -5.190390249166387804, 18.79952054102714598 ) ) ;
#5130 = CARTESIAN_POINT ( 'NONE',  ( 2.817313151351004130, -5.579000502529524397, 24.49999999999999289 ) ) ;
#5131 = CARTESIAN_POINT ( 'NONE',  ( 2.500000000000000444, 187.8499999978150470, 8.035533905932739529 ) ) ;
#5132 = CARTESIAN_POINT ( 'NONE',  ( 1.035533905932737975, 185.6499999978150868, 4.500000000000000888 ) ) ;
#5133 = CARTESIAN_POINT ( 'NONE',  ( -2.817313151351250156, 5.579000502529400940, 11.36765874365829099 ) ) ;
#5134 = CARTESIAN_POINT ( 'NONE',  ( -3.458467055437393078, 5.207305717053763772, 18.97359571723300320 ) ) ;
#5135 = PRODUCT_CONTEXT ( 'NONE', #12368, 'mechanical' ) ;
#5136 = CARTESIAN_POINT ( 'NONE',  ( 1.035533905932738419, 186.2199999975965738, 9.500000000000003553 ) ) ;
#5137 = CARTESIAN_POINT ( 'NONE',  ( -1.313542798833678749, 227.7708088449086290, 5.577473728656160645 ) ) ;
#5138 = CARTESIAN_POINT ( 'NONE',  ( -1.240485740468941556, 226.4108687305035232, 4.739277288743133809 ) ) ;
#5139 = EDGE_CURVE ( 'NONE', #8636, #4972, #14462, .T. ) ;
#5140 = CARTESIAN_POINT ( 'NONE',  ( -2.778918535561691439, 189.3544729152338846, 5.892260229556007367 ) ) ;
#5141 = ORIENTED_EDGE ( 'NONE', *, *, #6602, .T. ) ;
#5142 = CARTESIAN_POINT ( 'NONE',  ( -6.176542424588100211, 0.9554180641286806885, 17.99999999999998934 ) ) ;
#5143 = ADVANCED_FACE ( 'NONE', ( #7080 ), #15594, .F. ) ;
#5144 = DIRECTION ( 'NONE',  ( -1.000000000000000000, 0.000000000000000000, 0.000000000000000000 ) ) ;
#5145 = CARTESIAN_POINT ( 'NONE',  ( 0.7993401192312425962, -6.199366368793653770, 12.11483246936573721 ) ) ;
#5146 = CARTESIAN_POINT ( 'NONE',  ( 6.123233995736766282E-16, 2.000000000000000000, 5.000000000000000000 ) ) ;
#5147 = CARTESIAN_POINT ( 'NONE',  ( 2.999875809771047397, 227.2791568961600319, 7.297085794927967939 ) ) ;
#5148 = DIRECTION ( 'NONE',  ( -0.000000000000000000, 1.000000000000000000, -0.000000000000000000 ) ) ;
#5149 = CARTESIAN_POINT ( 'NONE',  ( -0.8561741729129455081, 2.066987299999999639, -2.699999998907525178 ) ) ;
#5150 = CARTESIAN_POINT ( 'NONE',  ( -2.997753866155991265, 5.484939622623749678, 23.88439807107078039 ) ) ;
#5151 = SURFACE_SIDE_STYLE ('',( #12613 ) ) ;
#5152 = CARTESIAN_POINT ( 'NONE',  ( 5.747343991580163625, 1.727858744772343247, 5.999920023562623328 ) ) ;
#5153 = CARTESIAN_POINT ( 'NONE',  ( 1.035533905932737975, 184.9499999999999886, 4.500000000000000888 ) ) ;
#5154 = CARTESIAN_POINT ( 'NONE',  ( -2.500000000000000000, 0.000000000000000000, -1.500000000000000000 ) ) ;
#5155 = CARTESIAN_POINT ( 'NONE',  ( 0.8230742150784297051, 227.6668866512619047, 5.277340506070477666 ) ) ;
#5156 = CARTESIAN_POINT ( 'NONE',  ( 2.066987299999999639, 2.531329380823229670E-16, -2.149999998907525356 ) ) ;
#5157 = VECTOR ( 'NONE', #13478, 1000.000000000000000 ) ;
#5158 = CARTESIAN_POINT ( 'NONE',  ( -3.255128505894268276, -5.336774832660745815, 10.62619944752603018 ) ) ;
#5159 = CARTESIAN_POINT ( 'NONE',  ( 1.461580736456473018, -1.461580736456472573, 1.550000001092474822 ) ) ;
#5160 = CARTESIAN_POINT ( 'NONE',  ( 0.8561741729129455081, 189.1999999989075434, 4.933012699999999029 ) ) ;
#5161 = CARTESIAN_POINT ( 'NONE',  ( -4.196038884587275142, 4.289036423669169373, 18.50389795015985328 ) ) ;
#5163 = VERTEX_POINT ( 'NONE', #12871 ) ;
#5162 = CARTESIAN_POINT ( 'NONE',  ( -5.421010862427522170E-16, 186.6499999989075320, 9.066987300000000971 ) ) ;
#5164 = LINE ( 'NONE', #6677, #7 ) ;
#5165 = CARTESIAN_POINT ( 'NONE',  ( 5.935543223013858949, -0.8771126767606638452, 5.000000000000004441 ) ) ;
#5166 = EDGE_CURVE ( 'NONE', #8072, #11236, #305, .T. ) ;
#5167 = CARTESIAN_POINT ( 'NONE',  ( -5.317509234263969375, 2.779225709350973350, 5.000000000000004441 ) ) ;
#5168 = CARTESIAN_POINT ( 'NONE',  ( -1.456896669277396583E-16, 188.4499999989075150, 4.933012699999999029 ) ) ;
#5169 = CARTESIAN_POINT ( 'NONE',  ( 4.005785023174365023, 4.467917056767481299, 17.20047945897285047 ) ) ;
#5170 = CARTESIAN_POINT ( 'NONE',  ( 2.471008584805455488, 189.0000000025389397, 6.581706668861207810 ) ) ;
#5171 = FACE_OUTER_BOUND ( 'NONE', #4869, .T. ) ;
#5172 = ADVANCED_FACE ( 'NONE', ( #7241 ), #145, .F. ) ;
#5173 = CARTESIAN_POINT ( 'NONE',  ( 2.266383616481251195, 189.7755269081602876, 9.339276568968184478 ) ) ;
#5174 = CARTESIAN_POINT ( 'NONE',  ( -2.500000000000000444, 1.035533905932737753, -2.249999997815050001 ) ) ;
#5175 = CARTESIAN_POINT ( 'NONE',  ( -5.935543223013836744, -0.8771126767608161678, 11.49999999999998224 ) ) ;
#5176 = CYLINDRICAL_SURFACE ( 'NONE', #14841, 1.000000000000000888 ) ;
#5177 = EDGE_LOOP ( 'NONE', ( #8765, #4731, #548, #8293 ) ) ;
#5178 = CARTESIAN_POINT ( 'NONE',  ( 0.8561741729129460632, 185.8999999989075036, 9.066987299999999195 ) ) ;
#5179 = ORIENTED_EDGE ( 'NONE', *, *, #15541, .F. ) ;
#5180 = CARTESIAN_POINT ( 'NONE',  ( -5.842988226680536634, 1.369004370660818370, 25.37380682714709579 ) ) ;
#5181 = B_SPLINE_CURVE_WITH_KNOTS ( 'NONE', 3,
 ( #14719, #6289, #8681, #2544, #14795, #7324, #7398, #5014, #12240, #12084, #11051, #6216, #3959, #73, #3650, #1262, #9868, #952, #13511, #7475, #12319, #6138 ),
 .UNSPECIFIED., .F., .F.,
 ( 4, 2, 2, 2, 2, 2, 2, 2, 2, 2, 4 ),
 ( 0.8845854629958906923, 0.9326205154887873272, 0.9806555679816839621, 1.028690620474580708, 1.052708146721028859, 1.076725672967477232, 1.124760725460373534, 1.148778251706821907, 1.172795777953270280, 1.220830830446166804, 1.268865882939063106 ),
 .UNSPECIFIED. ) ;
#5182 = VERTEX_POINT ( 'NONE', #10895 ) ;
#5183 = CARTESIAN_POINT ( 'NONE',  ( -2.849269941562166952, 5.281123252783936906, 25.11519382448850379 ) ) ;
#5184 = ORIENTED_EDGE ( 'NONE', *, *, #15661, .T. ) ;
#5185 = CARTESIAN_POINT ( 'NONE',  ( -0.8561741729129458411, -2.066987299999999195, 0.6000000010924746441 ) ) ;
#5186 = CARTESIAN_POINT ( 'NONE',  ( -3.459447313391850631, 5.206669755180985071, 4.025999019766706155 ) ) ;
#5187 = CARTESIAN_POINT ( 'NONE',  ( -0.9748673250649166899, 190.0717113996746264, 4.361044512588190258 ) ) ;
#5188 = LINE ( 'NONE', #3826, #2083 ) ;
#5189 = AXIS2_PLACEMENT_3D ( 'NONE', #9623, #13189, #7155 ) ;
#5190 = CARTESIAN_POINT ( 'NONE',  ( -1.767766952966369098, 1.767766952966369098, -2.393000000021849427 ) ) ;
#5191 = CARTESIAN_POINT ( 'NONE',  ( 0.000000000000000000, 202.2378330312726291, 13.30884679668974258 ) ) ;
#5192 = CONTEXT_DEPENDENT_SHAPE_REPRESENTATION ( #3486, #6793 ) ;
#5193 = CARTESIAN_POINT ( 'NONE',  ( -5.131373506000769247, 7.062729720843990755, 11.49999999999998224 ) ) ;
#5194 = CARTESIAN_POINT ( 'NONE',  ( 1.461580736456473018, -1.461580736456472573, 0.9500000010924747329 ) ) ;
#5195 = CARTESIAN_POINT ( 'NONE',  ( 2.668367453516629517, 5.373994336898132218, 5.000000000000004441 ) ) ;
#5196 = CARTESIAN_POINT ( 'NONE',  ( -0.9999505860953201708, 6.169489349035809589, 31.13105903165810773 ) ) ;
#5197 = ORIENTED_EDGE ( 'NONE', *, *, #10481, .T. ) ;
#5198 = B_SPLINE_CURVE_WITH_KNOTS ( 'NONE', 3,
 ( #2802, #14819, #2645, #4881, #5115, #13462, #12421, #9815, #10997, #97, #12264, #7497, #3674, #3752, #11230, #332, #174, #5038 ),
 .UNSPECIFIED., .F., .F.,
 ( 4, 2, 2, 2, 2, 2, 2, 2, 4 ),
 ( 0.000000000000000000, 0.0003914898357794947847, 0.0007829796715589895694, 0.001174469507338484191, 0.001565959343117978055, 0.001957449178897471918, 0.002348939014676965781, 0.002740428850456459644, 0.003131918686235953941 ),
 .UNSPECIFIED. ) ;
#5199 = ORIENTED_EDGE ( 'NONE', *, *, #9485, .F. ) ;
#5200 = ORIENTED_EDGE ( 'NONE', *, *, #2307, .F. ) ;
#5201 = CARTESIAN_POINT ( 'NONE',  ( 0.1323602877613519191, 6.000000000000000000, 18.99999999999998579 ) ) ;
#5202 = CARTESIAN_POINT ( 'NONE',  ( 4.344265632482118278, 4.493596842504927302, 4.495740504969913509 ) ) ;
#5203 = ORIENTED_EDGE ( 'NONE', *, *, #5922, .F. ) ;
#5204 = CARTESIAN_POINT ( 'NONE',  ( -6.176542424588101987, -0.9554180641286524889, 31.00000000000000000 ) ) ;
#5205 =( BOUNDED_SURFACE ( )  B_SPLINE_SURFACE ( 3, 3, ( 
 ( #12880, #15284, #4387, #9241, #2063, #8124, #15521, #6860 ),
 ( #11696, #14076, #11769, #11841, #10661, #15206, #14304, #5819 ),
 ( #2138, #15364, #3186, #10433, #5507, #11615, #1987, #14155 ),
 ( #796, #5739, #5662, #872, #7964, #14002, #3413, #4542 ),
 ( #10351, #10582, #4460, #13041, #9315, #9392, #3258, #14230 ),
 ( #4305, #3337, #951, #7011, #8205, #4620, #13118, #716 ),
 ( #8284, #9473, #2219, #7090, #1907, #9167, #3110, #12804 ) ),
 .UNSPECIFIED., .T., .F., .F. ) 
 B_SPLINE_SURFACE_WITH_KNOTS ( ( 4, 3, 4 ),
 ( 4, 2, 2, 4 ),
 ( 0.000000000000000000, 0.5000000000000000000, 1.000000000000000000 ),
 ( 0.000000000000000000, 0.05225677727458622607, 0.5261283886372931651, 1.000000000000000000 ),
 .UNSPECIFIED. ) 
 GEOMETRIC_REPRESENTATION_ITEM ( )  RATIONAL_B_SPLINE_SURFACE ( (
 ( 1.000000000000000000, 1.000000000000000000, 1.000000000000000000, 1.000000000000000000, 1.000000000000000000, 1.000000000000000000, 1.000000000000000000, 1.000000000000000000),
 ( 0.3333333333333333703, 0.3333333333333333703, 0.3333333333333333703, 0.3333333333333333703, 0.3333333333333333703, 0.3333333333333333703, 0.3333333333333333703, 0.3333333333333333703),
 ( 0.3333333333333333703, 0.3333333333333333703, 0.3333333333333333703, 0.3333333333333333703, 0.3333333333333333703, 0.3333333333333333703, 0.3333333333333333703, 0.3333333333333333703),
 ( 1.000000000000000000, 1.000000000000000000, 1.000000000000000000, 1.000000000000000000, 1.000000000000000000, 1.000000000000000000, 1.000000000000000000, 1.000000000000000000),
 ( 0.3333333333333333703, 0.3333333333333333703, 0.3333333333333333703, 0.3333333333333333703, 0.3333333333333333703, 0.3333333333333333703, 0.3333333333333333703, 0.3333333333333333703),
 ( 0.3333333333333333703, 0.3333333333333333703, 0.3333333333333333703, 0.3333333333333333703, 0.3333333333333333703, 0.3333333333333333703, 0.3333333333333333703, 0.3333333333333333703),
 ( 1.000000000000000000, 1.000000000000000000, 1.000000000000000000, 1.000000000000000000, 1.000000000000000000, 1.000000000000000000, 1.000000000000000000, 1.000000000000000000) ) ) 
 REPRESENTATION_ITEM ( '' )  SURFACE ( )  );
#5206 = CARTESIAN_POINT ( 'NONE',  ( 0.6139908388541118756, -5.969238533166610239, 30.19977627912011542 ) ) ;
#5207 = VECTOR ( 'NONE', #14931, 1000.000000000000114 ) ;
#5208 = EDGE_CURVE ( 'NONE', #4525, #7295, #7163, .T. ) ;
#5209 = CARTESIAN_POINT ( 'NONE',  ( -4.152999119458018029, 4.671604476854316346, 31.80026515017674882 ) ) ;
#5210 = CARTESIAN_POINT ( 'NONE',  ( 0.9737725088283790686, 6.173885267451797887, 17.73735758726570566 ) ) ;
#5211 = CARTESIAN_POINT ( 'NONE',  ( -2.500000000000000444, 185.8499999978150754, 5.964466094067261359 ) ) ;
#5212 = CARTESIAN_POINT ( 'NONE',  ( 2.500000000000000000, 3.061616997868383141E-16, 2.100000000000000089 ) ) ;
#5213 = CARTESIAN_POINT ( 'NONE',  ( 5.782895619916185836, -1.604017620857976167, 12.47408052783098853 ) ) ;
#5214 = B_SPLINE_CURVE_WITH_KNOTS ( 'NONE', 3,
 ( #7300, #4833, #8420, #8504, #1086, #11896, #2273, #13256, #9689, #14447, #2355, #12140, #7224, #1240, #14359, #4673 ),
 .UNSPECIFIED., .F., .F.,
 ( 4, 3, 3, 3, 3, 4 ),
 ( 8.915077171950578868E-05, 0.0001023483930351222872, 0.0001368170539646130666, 0.0001711500869964550833, 0.0002051216925220995921, 0.0002377972641794323314 ),
 .UNSPECIFIED. ) ;
#5215 = CARTESIAN_POINT ( 'NONE',  ( -4.344502777243645752, 4.493369211529153695, 18.50389213124969956 ) ) ;
#5216 = DIRECTION ( 'NONE',  ( 1.127570259384924611E-17, -1.000000000000000000, 0.000000000000000000 ) ) ;
#5217 = CARTESIAN_POINT ( 'NONE',  ( 2.500000000000000444, 187.2199999975966023, 5.964466094067262247 ) ) ;
#5218 = CARTESIAN_POINT ( 'NONE',  ( -1.914314807121730633, 228.0813985855225212, 6.474474614426593888 ) ) ;
#5219 = CARTESIAN_POINT ( 'NONE',  ( -1.329004440443209090, 226.4243434115648199, 4.778997713384572243 ) ) ;
#5220 =( BOUNDED_SURFACE ( )  B_SPLINE_SURFACE ( 3, 3, ( 
 ( #7473, #2460, #11050, #7323, #8605, #2618, #12163, #6137 ),
 ( #7166, #4938, #9790, #14639, #13439, #2543, #14387, #1107 ),
 ( #14718, #1340, #15676, #5971, #6215, #5013, #9632, #3807 ),
 ( #12318, #7782, #5250, #11360, #12472, #12629, #1573, #3957 ),
 ( #7629, #14868, #8832, #13662, #12552, #7704, #8753, #381 ),
 ( #9071, #6601, #14794, #1493, #10253, #3880, #13898, #5405 ),
 ( #1727, #14949, #2775, #11437, #10096, #13822, #15105, #13747 ) ),
 .UNSPECIFIED., .T., .F., .F. ) 
 B_SPLINE_SURFACE_WITH_KNOTS ( ( 4, 3, 4 ),
 ( 4, 2, 2, 4 ),
 ( 0.000000000000000000, 0.5000000000000000000, 1.000000000000000000 ),
 ( 0.000000000000000000, 0.05225677727458622607, 0.5261283886372931651, 1.000000000000000000 ),
 .UNSPECIFIED. ) 
 GEOMETRIC_REPRESENTATION_ITEM ( )  RATIONAL_B_SPLINE_SURFACE ( (
 ( 1.000000000000000000, 1.000000000000000000, 1.000000000000000000, 1.000000000000000000, 1.000000000000000000, 1.000000000000000000, 1.000000000000000000, 1.000000000000000000),
 ( 0.3333333333333333703, 0.3333333333333333703, 0.3333333333333333703, 0.3333333333333333703, 0.3333333333333333703, 0.3333333333333333703, 0.3333333333333333703, 0.3333333333333333703),
 ( 0.3333333333333333703, 0.3333333333333333703, 0.3333333333333333703, 0.3333333333333333703, 0.3333333333333333703, 0.3333333333333333703, 0.3333333333333333703, 0.3333333333333333703),
 ( 1.000000000000000000, 1.000000000000000000, 1.000000000000000000, 1.000000000000000000, 1.000000000000000000, 1.000000000000000000, 1.000000000000000000, 1.000000000000000000),
 ( 0.3333333333333333703, 0.3333333333333333703, 0.3333333333333333703, 0.3333333333333333703, 0.3333333333333333703, 0.3333333333333333703, 0.3333333333333333703, 0.3333333333333333703),
 ( 0.3333333333333333703, 0.3333333333333333703, 0.3333333333333333703, 0.3333333333333333703, 0.3333333333333333703, 0.3333333333333333703, 0.3333333333333333703, 0.3333333333333333703),
 ( 1.000000000000000000, 1.000000000000000000, 1.000000000000000000, 1.000000000000000000, 1.000000000000000000, 1.000000000000000000, 1.000000000000000000, 1.000000000000000000) ) ) 
 REPRESENTATION_ITEM ( '' )  SURFACE ( )  );
#5221 = EDGE_CURVE ( 'NONE', #8237, #8787, #8440, .T. ) ;
#5222 = CARTESIAN_POINT ( 'NONE',  ( -1.440803585010799637, 189.7277077271388919, 10.02067490447666920 ) ) ;
#5223 = ADVANCED_FACE ( 'NONE', ( #3646 ), #5009, .F. ) ;
#5224 = ORIENTED_EDGE ( 'NONE', *, *, #7474, .F. ) ;
#5225 = CARTESIAN_POINT ( 'NONE',  ( -6.155867707731101035, 1.081837891425948550, 17.49563030319846746 ) ) ;
#5226 = CARTESIAN_POINT ( 'NONE',  ( -3.061616997868391523E-16, 189.0000000000000000, -4.500000000000000888 ) ) ;
#5227 = CARTESIAN_POINT ( 'NONE',  ( -0.8738043859790733947, 6.188821459035875883, 5.503415602237494042 ) ) ;
#5228 = CARTESIAN_POINT ( 'NONE',  ( 6.172651332693083859, 0.9815532474594386159, 30.73809786915987630 ) ) ;
#5229 = CARTESIAN_POINT ( 'NONE',  ( 2.363458168944469584, 227.8848776677811827, 9.079507460819527864 ) ) ;
#5230 = MANIFOLD_SOLID_BREP ( 'Thread1', #12830 ) ;
#5231 = CARTESIAN_POINT ( 'NONE',  ( -3.567258970015910080, -5.133675764669719754, 32.00008219321556169 ) ) ;
#5232 = CARTESIAN_POINT ( 'NONE',  ( -1.035533905932737753, 2.500000000000000444, 2.350000000000000533 ) ) ;
#5233 = CARTESIAN_POINT ( 'NONE',  ( 4.267558728637196097, 4.217879122113799895, 4.736173967944048435 ) ) ;
#5234 = FILL_AREA_STYLE_COLOUR ( '', #11177 ) ;
#5235 = CARTESIAN_POINT ( 'NONE',  ( 7.180990026460762010, -3.384707322287334286, 11.49999999999998224 ) ) ;
#5236 = CARTESIAN_POINT ( 'NONE',  ( -2.500000000000000444, 185.2499999999999716, 8.035533905932737753 ) ) ;
#5237 = FACE_BOUND ( 'NONE', #6967, .T. ) ;
#5238 = EDGE_CURVE ( 'NONE', #8865, #5590, #1771, .T. ) ;
#5239 = CARTESIAN_POINT ( 'NONE',  ( 0.5174937098143853609, 227.6312805367891201, 5.174508016632918483 ) ) ;
#5240 = CARTESIAN_POINT ( 'NONE',  ( 1.461580736456472573, 1.461580736456472795, -2.049999998907525267 ) ) ;
#5241 = CARTESIAN_POINT ( 'NONE',  ( 6.172651332693125603, -0.9815532474591706080, 24.76190213084012726 ) ) ;
#5242 = CYLINDRICAL_SURFACE ( 'NONE', #6310, 1.499999999999999556 ) ;
#5243 = CARTESIAN_POINT ( 'NONE',  ( -1.035533905932739529, 184.5499999999999829, 9.500000000000003553 ) ) ;
#5244 = CARTESIAN_POINT ( 'NONE',  ( 5.940390500375443139, 6.474944468551700361, 17.99999999999998934 ) ) ;
#5245 = ADVANCED_FACE ( 'NONE', ( #4935 ), #14636, .T. ) ;
#5247 = VERTEX_POINT ( 'NONE', #2540 ) ;
#5246 = CARTESIAN_POINT ( 'NONE',  ( -1.084202172485504434E-16, 187.8499999989074922, 4.933012699999999029 ) ) ;
#5248 = CARTESIAN_POINT ( 'NONE',  ( -3.158825713737554164, -5.393784879207130345, 17.20066851092422411 ) ) ;
#5249 = CARTESIAN_POINT ( 'NONE',  ( 6.105747081304188306, -1.338335777572190466, 12.30026515017674882 ) ) ;
#5250 = CARTESIAN_POINT ( 'NONE',  ( 3.659182332138577465E-16, 189.3270225533669020, 3.938484906660876472 ) ) ;
#5251 = DIRECTION ( 'NONE',  ( -0.5877852522924685852, -0.8090169943749507819, 0.000000000000000000 ) ) ;
#5252 = CARTESIAN_POINT ( 'NONE',  ( 2.668367453516444776, 5.373994336898222812, 24.49999999999999289 ) ) ;
#5253 = CARTESIAN_POINT ( 'NONE',  ( 2.943069445653888838, 189.3294980521935997, 6.426540498107687682 ) ) ;
#5254 = CARTESIAN_POINT ( 'NONE',  ( 0.05368748911329641882, -0.3999999999999923617, -2.541415605245799902 ) ) ;
#5255 = CARTESIAN_POINT ( 'NONE',  ( 2.782156709077490131, -5.316215864844006767, 5.503120489023789474 ) ) ;
#5256 = CARTESIAN_POINT ( 'NONE',  ( -3.634089073485446963, 4.776071126502678510, 30.00007997643739088 ) ) ;
#5257 = CARTESIAN_POINT ( 'NONE',  ( 0.4244143561419055910, -0.3999999999999975797, 2.581346380257588891 ) ) ;
#5258 = CARTESIAN_POINT ( 'NONE',  ( -1.768703179866833342, 189.0000639513403939, 5.233169770031948609 ) ) ;
#5259 = VERTEX_POINT ( 'NONE', #8676 ) ;
#5260 = CARTESIAN_POINT ( 'NONE',  ( 1.461580736456473018, 186.1499999989075320, 5.538419263543527649 ) ) ;
#5261 = ADVANCED_FACE ( 'NONE', ( #12312 ), #1410, .F. ) ;
#5262 = ORIENTED_EDGE ( 'NONE', *, *, #12407, .F. ) ;
#5263 = FACE_OUTER_BOUND ( 'NONE', #11388, .T. ) ;
#5264 = VERTEX_POINT ( 'NONE', #379 ) ;
#5265 = CARTESIAN_POINT ( 'NONE',  ( -3.061616997868391523E-16, 189.0000000000000000, -7.000000000000000000 ) ) ;
#5266 =( NAMED_UNIT ( * ) PLANE_ANGLE_UNIT ( ) SI_UNIT ( $, .RADIAN. ) );
#5267 = AXIS2_PLACEMENT_3D ( 'NONE', #1715, #14198, #11426 ) ;
#5268 = VERTEX_POINT ( 'NONE', #11280 ) ;
#5269 = CARTESIAN_POINT ( 'NONE',  ( -1.461580736456472351, -1.461580736456473018, 0.5500000010924748217 ) ) ;
#5270 = CARTESIAN_POINT ( 'NONE',  ( -0.8736516769105580060, 5.936271176698252106, 17.49606771578676145 ) ) ;
#5271 = CARTESIAN_POINT ( 'NONE',  ( -0.6743670111594756156, 228.2309373833427344, 10.09717849966832226 ) ) ;
#5272 = CARTESIAN_POINT ( 'NONE',  ( -2.066987300000001415, 188.8999999989075320, 7.856174172912944620 ) ) ;
#5273 = CARTESIAN_POINT ( 'NONE',  ( -2.500000000000000444, 1.035533905932737753, 1.750000002184949999 ) ) ;
#5274 = CARTESIAN_POINT ( 'NONE',  ( -2.500000000000000444, 1.035533905932737753, 2.449999999999999734 ) ) ;
#5275 = DIRECTION ( 'NONE',  ( 0.000000000000000000, 0.000000000000000000, -1.000000000000000000 ) ) ;
#5276 = CARTESIAN_POINT ( 'NONE',  ( 0.000000000000000000, 182.0000000000000000, 0.000000000000000000 ) ) ;
#5277 = CARTESIAN_POINT ( 'NONE',  ( 0.8561741729129463963, -2.066987299999999195, -1.499999998907525445 ) ) ;
#5278 = DIRECTION ( 'NONE',  ( 0.000000000000000000, 0.000000000000000000, 1.000000000000000000 ) ) ;
#5279 = CARTESIAN_POINT ( 'NONE',  ( 3.922288969639730727, 4.542045818322569595, 12.37378430870260715 ) ) ;
#5280 = AXIS2_PLACEMENT_3D ( 'NONE', #1479, #3789, #11113 ) ;
#5281 = ORIENTED_EDGE ( 'NONE', *, *, #7474, .T. ) ;
#5282 = EDGE_CURVE ( 'NONE', #13328, #8099, #14748, .T. ) ;
#5283 = EDGE_LOOP ( 'NONE', ( #14465, #14145 ) ) ;
#5284 = ORIENTED_EDGE ( 'NONE', *, *, #474, .F. ) ;
#5285 = CARTESIAN_POINT ( 'NONE',  ( 0.9999196734184028212, 5.916093360767494147, 17.86725955955069622 ) ) ;
#5286 = DIRECTION ( 'NONE',  ( -0.000000000000000000, 1.000000000000000000, -0.000000000000000000 ) ) ;
#5287 = ORIENTED_EDGE ( 'NONE', *, *, #1564, .F. ) ;
#5288 = ORIENTED_EDGE ( 'NONE', *, *, #1535, .F. ) ;
#5289 = CARTESIAN_POINT ( 'NONE',  ( -5.615811513734942473, -2.743665920700590011, 17.49691356133953590 ) ) ;
#5290 = CARTESIAN_POINT ( 'NONE',  ( 0.8738043859791964074, -6.188821459035860784, 18.50341560223750648 ) ) ;
#5291 = AXIS2_PLACEMENT_3D ( 'NONE', #2559, #6232, #14492 ) ;
#5292 = CARTESIAN_POINT ( 'NONE',  ( -4.435347140101089103, 4.403429997944455110, 31.00000000000000000 ) ) ;
#5293 = CARTESIAN_POINT ( 'NONE',  ( 5.616116467183648098, -2.743044348085566408, 30.49574050496988775 ) ) ;
#5294 = CARTESIAN_POINT ( 'NONE',  ( -1.767766952966369542, 185.9999999978150527, 8.767766952966368876 ) ) ;
#5295 = CARTESIAN_POINT ( 'NONE',  ( -1.035533905932737753, 2.500000000000000444, 2.356999999978150573 ) ) ;
#5296 = CARTESIAN_POINT ( 'NONE',  ( 2.030576276931546336E-13, -6.250000000000000888, 25.49999999999999645 ) ) ;
#5297 =( NAMED_UNIT ( * ) SI_UNIT ( $, .STERADIAN. ) SOLID_ANGLE_UNIT ( ) );
#5298 = CARTESIAN_POINT ( 'NONE',  ( -1.035533905932739751, 187.7199999975965738, 9.500000000000003553 ) ) ;
#5299 = CARTESIAN_POINT ( 'NONE',  ( 0.7764192831524953098, 228.2223555856212442, 10.07190823357606213 ) ) ;
#5300 = CARTESIAN_POINT ( 'NONE',  ( -2.960186505457850892, 227.4470585832885661, 7.791309201570119747 ) ) ;
#5301 = VECTOR ( 'NONE', #62, 1000.000000000000114 ) ;
#5302 = VERTEX_POINT ( 'NONE', #13745 ) ;
#5303 = AXIS2_PLACEMENT_3D ( 'NONE', #6703, #11614, #15049 ) ;
#5304 = CARTESIAN_POINT ( 'NONE',  ( -2.994879556239296026, 189.2754426180449343, 7.463391921200928536 ) ) ;
#5305 = SHAPE_REPRESENTATION ( 'pneumatic air inlet fitting', ( #14201 ), #6617 ) ;
#5306 = ORIENTED_EDGE ( 'NONE', *, *, #586, .F. ) ;
#5307 = DIRECTION ( 'NONE',  ( 0.000000000000000000, 0.000000000000000000, 1.000000000000000000 ) ) ;
#5308 = CARTESIAN_POINT ( 'NONE',  ( -5.770167736194656172, 2.404664418229267575, 23.62632671364006853 ) ) ;
#5309 = CARTESIAN_POINT ( 'NONE',  ( 4.435347140100977192, -4.403429997944567020, 17.99999999999998934 ) ) ;
#5310 = CARTESIAN_POINT ( 'NONE',  ( 6.081836621194437242, 1.445163676684838361, 12.37305891554298931 ) ) ;
#5311 = CARTESIAN_POINT ( 'NONE',  ( 2.805029955784917206, 227.6318923565098942, 8.335241701881683341 ) ) ;
#5312 = VECTOR ( 'NONE', #8096, 1000.000000000000000 ) ;
#5313 = FACE_BOUND ( 'NONE', #9154, .T. ) ;
#5314 = CARTESIAN_POINT ( 'NONE',  ( -2.066987299999999195, -0.8561741729129466183, -1.699999998907525400 ) ) ;
#5315 = LINE ( 'NONE', #11420, #7927 ) ;
#5316 = CARTESIAN_POINT ( 'NONE',  ( -3.779082820360620598, -4.979770177899308869, 29.99995093123466816 ) ) ;
#5317 = CARTESIAN_POINT ( 'NONE',  ( -1.035533905932737975, 187.4499999999999886, 4.500000000000000888 ) ) ;
#5318 = CARTESIAN_POINT ( 'NONE',  ( 1.362382138968808887, 227.7849605967929847, 5.618344795260735935 ) ) ;
#5319 = CARTESIAN_POINT ( 'NONE',  ( -2.817313151351206635, 5.579000502529421368, 31.00000000000000000 ) ) ;
#5320 = CARTESIAN_POINT ( 'NONE',  ( 4.435347140100959429, 4.403429997944583008, 11.63237410716304332 ) ) ;
#5321 = CARTESIAN_POINT ( 'NONE',  ( 0.8499999999999896527, 0.000000000000000000, 0.000000000000000000 ) ) ;
#5322 = CIRCLE ( 'NONE', #13186, 1.499999999999999556 ) ;
#5323 = CARTESIAN_POINT ( 'NONE',  ( 1.767766952966368654, 184.7000000000000171, 8.767766952966368876 ) ) ;
#5324 = CARTESIAN_POINT ( 'NONE',  ( -3.011139120916648260, 5.190534000030265105, 18.79931806258173665 ) ) ;
#5326 = ORIENTED_EDGE ( 'NONE', *, *, #5914, .T. ) ;
#5325 = CARTESIAN_POINT ( 'NONE',  ( 2.066987299999999639, 188.4499999989075150, 7.000000000000000000 ) ) ;
#5327 = CARTESIAN_POINT ( 'NONE',  ( -4.070051655338138730, -4.744673454622449604, 17.12632671364005787 ) ) ;
#5328 = EDGE_CURVE ( 'NONE', #13528, #7812, #12808, .T. ) ;
#5329 = EDGE_CURVE ( 'NONE', #1423, #6465, #10934, .T. ) ;
#5330 = DIRECTION ( 'NONE',  ( -6.123233995736766036E-17, 1.000000000000000000, 0.000000000000000000 ) ) ;
#5331 = EDGE_CURVE ( 'NONE', #7351, #2035, #5164, .T. ) ;
#5332 = CARTESIAN_POINT ( 'NONE',  ( -5.746837578676025515, 1.729433780394186382, 4.000049463537776795 ) ) ;
#5333 =( GEOMETRIC_REPRESENTATION_CONTEXT ( 3 ) GLOBAL_UNCERTAINTY_ASSIGNED_CONTEXT ( ( #13155 ) ) GLOBAL_UNIT_ASSIGNED_CONTEXT ( ( #538, #13981, #1806 ) ) REPRESENTATION_CONTEXT ( 'NONE', 'WORKASPACE' ) );
#5334 = CARTESIAN_POINT ( 'NONE',  ( 2.596699584268322258, 189.8036601807143313, 8.865069138243688585 ) ) ;
#5335 = FACE_OUTER_BOUND ( 'NONE', #6714, .T. ) ;
#5336 = FACE_OUTER_BOUND ( 'NONE', #12809, .T. ) ;
#5337 = CARTESIAN_POINT ( 'NONE',  ( 5.616089948629725548, -2.743103014345551482, 5.504369696801525436 ) ) ;
#5338 = DIRECTION ( 'NONE',  ( 0.000000000000000000, 1.000000000000000000, 0.000000000000000000 ) ) ;
#5339 = CARTESIAN_POINT ( 'NONE',  ( 0.000000000000000000, 19.99999999999999645, 0.000000000000000000 ) ) ;
#5340 = EDGE_LOOP ( 'NONE', ( #4910, #5511, #14806, #14609 ) ) ;
#5341 = CARTESIAN_POINT ( 'NONE',  ( -2.066987300000000527, 188.0499999989075093, 7.000000000000000000 ) ) ;
#5342 = ORIENTED_EDGE ( 'NONE', *, *, #1035, .F. ) ;
#5343 = DIRECTION ( 'NONE',  ( -1.000000000000000000, 0.000000000000000000, 0.000000000000000000 ) ) ;
#5344 = VERTEX_POINT ( 'NONE', #12470 ) ;
#5345 = CARTESIAN_POINT ( 'NONE',  ( 0.000000000000000000, 2.000000000000000000, 0.000000000000000000 ) ) ;
#5346 = CARTESIAN_POINT ( 'NONE',  ( -3.061616997868391523E-16, 182.0000000000000000, -4.500000000000000888 ) ) ;
#5347 = VECTOR ( 'NONE', #13873, 1000.000000000000114 ) ;
#5348 = VERTEX_POINT ( 'NONE', #7701 ) ;
#5349 = CARTESIAN_POINT ( 'NONE',  ( -3.736532060717933756, -4.696070028786013317, 5.973778239432933290 ) ) ;
#5350 = CARTESIAN_POINT ( 'NONE',  ( -3.118365096457674568, 189.0000000000000000, 7.000000000000000888 ) ) ;
#5351 = CARTESIAN_POINT ( 'NONE',  ( 2.066987299999999639, 189.2499999989075263, 7.000000000000000000 ) ) ;
#5352 = CARTESIAN_POINT ( 'NONE',  ( -1.035533905932737753, 2.500000000000000444, -0.8500000000000001998 ) ) ;
#5353 = CARTESIAN_POINT ( 'NONE',  ( -5.726307184802639227, -2.506131700382496330, 5.800265150176761253 ) ) ;
#5354 = CARTESIAN_POINT ( 'NONE',  ( -2.849573632035372839, 5.280958870664546723, 17.38438267301393481 ) ) ;
#5355 = CONTEXT_DEPENDENT_SHAPE_REPRESENTATION ( #15447, #11733 ) ;
#5356 = AXIS2_PLACEMENT_3D ( 'NONE', #14763, #14517, #11968 ) ;
#5357 = CARTESIAN_POINT ( 'NONE',  ( -2.500000000000000444, 1.035533905932737753, -0.6499999978150501345 ) ) ;
#5358 = CARTESIAN_POINT ( 'NONE',  ( -0.8561741729129458411, -2.066987299999999195, -1.599999998907525534 ) ) ;
#5359 = CARTESIAN_POINT ( 'NONE',  ( 4.195842658231422995, 4.289229542213213620, 12.00439760644213294 ) ) ;
#5360 = ORIENTED_EDGE ( 'NONE', *, *, #460, .T. ) ;
#5361 = EDGE_LOOP ( 'NONE', ( #315, #15554, #5044, #1370 ) ) ;
#5362 = EDGE_LOOP ( 'NONE', ( #2793, #84, #11396, #7123 ) ) ;
#5363 = EDGE_CURVE ( 'NONE', #12662, #8844, #3007, .T. ) ;
#5364 = CARTESIAN_POINT ( 'NONE',  ( 3.566234721238094707, -5.134387337253790484, 12.49991741810287138 ) ) ;
#5365 = CARTESIAN_POINT ( 'NONE',  ( 5.984377695197210301, 1.807429553002331879, 3.999950931234676599 ) ) ;
#5366 = ORIENTED_EDGE ( 'NONE', *, *, #13936, .F. ) ;
#5367 = SURFACE_STYLE_USAGE ( .BOTH. , #10443 ) ;
#5368 = LINE ( 'NONE', #12354, #3600 ) ;
#5369 = CARTESIAN_POINT ( 'NONE',  ( -5.531209434046362894, 2.328189801702562178, 5.873037790270514868 ) ) ;
#5370 = CARTESIAN_POINT ( 'NONE',  ( -1.767766952966368432, -1.767766952966369320, -2.200000000000000178 ) ) ;
#5371 = CARTESIAN_POINT ( 'NONE',  ( -1.035533905932739751, 186.8499999978150470, 9.500000000000003553 ) ) ;
#5372 = ADVANCED_FACE ( 'NONE', ( #6447 ), #15178, .F. ) ;
#5373 = CARTESIAN_POINT ( 'NONE',  ( -2.500000000000000000, -0.4783542904563624076, 2.530096988290932547 ) ) ;
#5374 = CARTESIAN_POINT ( 'NONE',  ( 4.286401442266485340, 4.198423832313245008, 11.36763921416086554 ) ) ;
#5375 = CARTESIAN_POINT ( 'NONE',  ( 1.035533905932738419, 185.4199999975965909, 9.500000000000003553 ) ) ;
#5376 = CARTESIAN_POINT ( 'NONE',  ( -1.724643626337419855, 228.5864753960848077, 7.933165251024266063 ) ) ;
#5377 = ADVANCED_FACE ( 'NONE', ( #13658, #7865, #12705, #12550, #15026, #13818 ), #1647, .F. ) ;
#5378 = CARTESIAN_POINT ( 'NONE',  ( -2.842542329930219491, 227.5997332721124451, 8.240608773874100734 ) ) ;
#5379 = ORIENTED_EDGE ( 'NONE', *, *, #14202, .T. ) ;
#5380 = CARTESIAN_POINT ( 'NONE',  ( 2.236053883310440860, -1.154369717630873149, -2.500600154548837217 ) ) ;
#5381 = VERTEX_POINT ( 'NONE', #8015 ) ;
#5382 = CARTESIAN_POINT ( 'NONE',  ( -3.255013540813745720, 5.336859797930771698, 17.12618035954928075 ) ) ;
#5383 = B_SPLINE_CURVE_WITH_KNOTS ( 'NONE', 3,
 ( #11958, #10932, #8314, #9505, #14340, #1064, #7202, #15714, #13070, #5847, #1141, #9584, #14427, #6171, #3445, #12043, #3531, #1220 ),
 .UNSPECIFIED., .F., .F.,
 ( 4, 2, 2, 2, 2, 2, 2, 2, 4 ),
 ( 0.003131918686235977359, 0.003523310662250266762, 0.003914702638264556597, 0.004306094614278846433, 0.004697486590293137136, 0.005088878566307427839, 0.005480270542321717675, 0.005871662518336009245, 0.006263054494350299081 ),
 .UNSPECIFIED. ) ;
#5384 = CARTESIAN_POINT ( 'NONE',  ( 3.459597053047867465, -5.206576120509730288, 10.52591457665827157 ) ) ;
#5385 = CARTESIAN_POINT ( 'NONE',  ( 7.347881158177969135E-16, 6.250000000000000888, 4.000000000000004441 ) ) ;
#5386 = CARTESIAN_POINT ( 'NONE',  ( 5.558508435838221295, 2.857531096718872288, 11.63234125634166105 ) ) ;
#5387 = CARTESIAN_POINT ( 'NONE',  ( 2.794738844873451811, 227.6405336420577896, 8.360663504027472825 ) ) ;
#5388 = CARTESIAN_POINT ( 'NONE',  ( 3.779681992289804615, 4.979315417303895153, 5.999950789842940502 ) ) ;
#5389 = CARTESIAN_POINT ( 'NONE',  ( -4.416678568553731310, -4.422441866694230228, 18.26236973443872813 ) ) ;
#5390 = CARTESIAN_POINT ( 'NONE',  ( 2.066987299999999639, 0.8561741729129456191, -1.299999998907525267 ) ) ;
#5391 = CARTESIAN_POINT ( 'NONE',  ( -4.006441409774673446, -4.467329318258270732, 31.79888242247941221 ) ) ;
#5392 = FACE_OUTER_BOUND ( 'NONE', #7719, .T. ) ;
#5393 = CARTESIAN_POINT ( 'NONE',  ( -1.035533905932739751, 186.1500000000000057, 9.500000000000003553 ) ) ;
#5394 = CARTESIAN_POINT ( 'NONE',  ( -1.580027211161896261, 227.8635840621947182, 5.845413847729996171 ) ) ;
#5395 = FACE_BOUND ( 'NONE', #27, .T. ) ;
#5396 = CARTESIAN_POINT ( 'NONE',  ( -3.158825713737495544, -5.393784879207164096, 10.70066851092422411 ) ) ;
#5397 = CARTESIAN_POINT ( 'NONE',  ( -1.265664690411614835E-16, 2.066987299999999639, -0.5499999989075254891 ) ) ;
#5398 = AXIS2_PLACEMENT_3D ( 'NONE', #4896, #13314, #2255 ) ;
#5399 = CARTESIAN_POINT ( 'NONE',  ( -2.500000000000000444, 185.1500000000000057, 5.964466094067261359 ) ) ;
#5400 = CARTESIAN_POINT ( 'NONE',  ( -2.668367453516831134, 5.373994336898032742, 17.99999999999998934 ) ) ;
#5402 = ORIENTED_EDGE ( 'NONE', *, *, #2616, .F. ) ;
#5401 = CARTESIAN_POINT ( 'NONE',  ( 1.461580736456472795, 186.9499999989075150, 5.538419263543527649 ) ) ;
#5403 = CARTESIAN_POINT ( 'NONE',  ( -3.255128505894326008, -5.336774832660711176, 17.12619944752603729 ) ) ;
#5404 = CARTESIAN_POINT ( 'NONE',  ( 5.931793676715114927, -0.9035324301687286397, 17.73760108194402108 ) ) ;
#5405 = CARTESIAN_POINT ( 'NONE',  ( -5.999999999999999112, 229.2449477060184222, 9.834870838912449287 ) ) ;
#5406 = DIRECTION ( 'NONE',  ( 0.000000000000000000, 0.000000000000000000, 1.000000000000000000 ) ) ;
#5407 = VECTOR ( 'NONE', #13403, 1000.000000000000000 ) ;
#5408 = CARTESIAN_POINT ( 'NONE',  ( 2.388242814291142047, 188.9999999974610603, 6.240296794481074549 ) ) ;
#5409 = DIRECTION ( 'NONE',  ( 0.5877852522924802425, -0.8090169943749422332, 0.000000000000000000 ) ) ;
#5410 = CARTESIAN_POINT ( 'NONE',  ( 2.094888807778566729E-14, 6.000000000000000888, 30.00000000000000000 ) ) ;
#5411 = CARTESIAN_POINT ( 'NONE',  ( 4.195795028115118619, -4.289273350251234795, 5.504289203620184701 ) ) ;
#5412 = CARTESIAN_POINT ( 'NONE',  ( -4.196288036172437508, 4.288789315524846657, 30.49687951097621763 ) ) ;
#5413 = DIRECTION ( 'NONE',  ( 0.8090169943749506709, -0.5877852522924689183, 0.000000000000000000 ) ) ;
#5414 = CARTESIAN_POINT ( 'NONE',  ( -2.500000000000000444, 186.7999999999999829, 7.000000000000000000 ) ) ;
#5415 = ORIENTED_EDGE ( 'NONE', *, *, #2836, .F. ) ;
#5416 = CARTESIAN_POINT ( 'NONE',  ( -1.461580736456473018, 187.1499999989075320, 5.538419263543527649 ) ) ;
#5417 = EDGE_CURVE ( 'NONE', #12389, #13930, #12955, .T. ) ;
#5418 = VERTEX_POINT ( 'NONE', #12855 ) ;
#5419 = CARTESIAN_POINT ( 'NONE',  ( -5.375605342016400279, -2.665598297262502303, 23.99687951097623184 ) ) ;
#5420 = EDGE_LOOP ( 'NONE', ( #4468, #9881 ) ) ;
#5421 = AXIS2_PLACEMENT_3D ( 'NONE', #6879, #10450, #4406 ) ;
#5422 = FACE_OUTER_BOUND ( 'NONE', #8693, .T. ) ;
#5423 = DIRECTION ( 'NONE',  ( 0.000000000000000000, 1.000000000000000000, 0.000000000000000000 ) ) ;
#5424 = EDGE_CURVE ( 'NONE', #12389, #3604, #15337, .T. ) ;
#5425 = CARTESIAN_POINT ( 'NONE',  ( 2.066987299999999639, 2.531329380823229670E-16, -2.349999998907525534 ) ) ;
#5426 = CARTESIAN_POINT ( 'NONE',  ( -0.9735856429311440241, 5.920699391845048787, 18.26285283906727486 ) ) ;
#5427 = CARTESIAN_POINT ( 'NONE',  ( -0.9999505860951506397, 6.169489349035837122, 24.63105903165801180 ) ) ;
#5428 = CARTESIAN_POINT ( 'NONE',  ( 1.767766952966368654, 1.767766952966369098, -0.2000000000000000944 ) ) ;
#5429 = CARTESIAN_POINT ( 'NONE',  ( -2.500000000000000000, 0.000000000000000000, -0.7000000000000000666 ) ) ;
#5430 = CARTESIAN_POINT ( 'NONE',  ( 0.000000000000000000, 184.0000000000000000, 0.000000000000000000 ) ) ;
#5431 = CARTESIAN_POINT ( 'NONE',  ( -6.437450399132682577E-16, 187.0000000000000000, 9.500000000000001776 ) ) ;
#5432 = CARTESIAN_POINT ( 'NONE',  ( 2.066987300000000083, -0.8561741729129449530, 1.000000001092474777 ) ) ;
#5433 = CARTESIAN_POINT ( 'NONE',  ( 1.767766952966369320, 186.3999999978150584, 5.232233047033630235 ) ) ;
#5434 = ADVANCED_FACE ( 'NONE', ( #3316 ), #13094, .F. ) ;
#5435 = ORIENTED_EDGE ( 'NONE', *, *, #11555, .F. ) ;
#5436 = ORIENTED_EDGE ( 'NONE', *, *, #8359, .F. ) ;
#5437 = ORIENTED_EDGE ( 'NONE', *, *, #2729, .F. ) ;
#5438 = CARTESIAN_POINT ( 'NONE',  ( 2.841163418881348601, -5.567120626447951359, 18.26236973443873524 ) ) ;
#5439 = DIRECTION ( 'NONE',  ( 0.000000000000000000, 1.000000000000000000, 0.000000000000000000 ) ) ;
#5440 = EDGE_CURVE ( 'NONE', #14829, #8273, #1958, .T. ) ;
#5441 = EDGE_LOOP ( 'NONE', ( #9445, #6963, #3343, #10496 ) ) ;
#5442 = DIRECTION ( 'NONE',  ( 0.000000000000000000, 0.000000000000000000, 1.000000000000000000 ) ) ;
#5443 = AXIS2_PLACEMENT_3D ( 'NONE', #6766, #11683, #5571 ) ;
#5444 = CARTESIAN_POINT ( 'NONE',  ( -2.500000000000000000, 0.000000000000000000, 1.800000002184949599 ) ) ;
#5445 = CARTESIAN_POINT ( 'NONE',  ( -5.782947755040686033, 1.603807858343911930, 5.973980201222398811 ) ) ;
#5446 = CARTESIAN_POINT ( 'NONE',  ( 1.035533905932739085, -2.500000000000000000, -2.050000000000000266 ) ) ;
#5447 = CARTESIAN_POINT ( 'NONE',  ( -2.500000000000000444, 188.2499999978150242, 5.964466094067261359 ) ) ;
#5448 = CARTESIAN_POINT ( 'NONE',  ( 5.915699123067175158, -1.003533581835451383, 12.00389795015984973 ) ) ;
#5449 = ADVANCED_FACE ( 'NONE', ( #7062 ), #5790, .F. ) ;
#5450 = CARTESIAN_POINT ( 'NONE',  ( 4.195795028115012926, 4.289273350251342265, 10.99571079637980908 ) ) ;
#5451 = DIRECTION ( 'NONE',  ( 0.000000000000000000, -1.000000000000000000, 0.000000000000000000 ) ) ;
#5452 = CARTESIAN_POINT ( 'NONE',  ( 1.035533905932737753, 188.1199999975965511, 4.500000000000000888 ) ) ;
#5453 = CARTESIAN_POINT ( 'NONE',  ( 0.3900692251286368428, 228.2474522196246767, 10.14569219465573546 ) ) ;
#5454 = CARTESIAN_POINT ( 'NONE',  ( -2.922039326512111401, 227.0704416020563201, 6.682560001249291837 ) ) ;
#5455 = EDGE_LOOP ( 'NONE', ( #1211, #4792 ) ) ;
#5456 = CARTESIAN_POINT ( 'NONE',  ( -0.5677240627250873528, 2.451883390204808055, -2.500792191741393555 ) ) ;
#5457 = ADVANCED_FACE ( 'NONE', ( #13978 ), #10405, .F. ) ;
#5458 = VERTEX_POINT ( 'NONE', #7932 ) ;
#5459 = CARTESIAN_POINT ( 'NONE',  ( -0.9735954530124610873, 6.173909381474003588, 11.76281793585240898 ) ) ;
#5460 = CIRCLE ( 'NONE', #5707, 1.499999999999999556 ) ;
#5461 = CARTESIAN_POINT ( 'NONE',  ( 4.195842658231450528, -4.289229542213186086, 17.49560239355786706 ) ) ;
#5462 = CARTESIAN_POINT ( 'NONE',  ( 0.8561741729129458411, 184.3999999989075036, 4.933012699999999029 ) ) ;
#5463 = CYLINDRICAL_SURFACE ( 'NONE', #8884, 1.500000000000000000 ) ;
#5464 = CARTESIAN_POINT ( 'NONE',  ( 2.841163418881336167, 5.567120626447958465, 11.23763026556121680 ) ) ;
#5465 = EDGE_CURVE ( 'NONE', #14081, #13047, #10371, .T. ) ;
#5466 = CARTESIAN_POINT ( 'NONE',  ( -4.290821322214338096, -4.545321419741590319, 31.61441947245485196 ) ) ;
#5467 = DIRECTION ( 'NONE',  ( 0.000000000000000000, 0.000000000000000000, -1.000000000000000000 ) ) ;
#5468 = B_SPLINE_CURVE_WITH_KNOTS ( 'NONE', 3,
 ( #7492, #14739, #7722, #4140, #8775, #13606, #8121, #14227, #5427, #5735, #1984, #10579, #12877, #7802, #6857, #793, #13998, #11693 ),
 .UNSPECIFIED., .F., .F.,
 ( 4, 2, 2, 2, 2, 2, 2, 2, 4 ),
 ( 0.000000000000000000, 0.0003914362731607349145, 0.0007828725463214698289, 0.001174308819482204743, 0.001565745092642939658, 0.001957181365803674356, 0.002348617638964409487, 0.002740053912125144618, 0.003131490185285879316 ),
 .UNSPECIFIED. ) ;
#5469 = CARTESIAN_POINT ( 'NONE',  ( -2.500000000000000000, 0.000000000000000000, -0.7000000000000000666 ) ) ;
#5470 = CARTESIAN_POINT ( 'NONE',  ( -4.142620314836317874, -4.341347824677564304, 31.61442521571936837 ) ) ;
#5471 = CARTESIAN_POINT ( 'NONE',  ( 1.734723475976807094E-15, 2.000000000000000000, 13.50000000000000000 ) ) ;
#5472 = CARTESIAN_POINT ( 'NONE',  ( 2.500000000000000444, 186.4500000000000171, 5.964466094067262247 ) ) ;
#5473 = AXIS2_PLACEMENT_3D ( 'NONE', #5642, #3167, #14138 ) ;
#5474 = CARTESIAN_POINT ( 'NONE',  ( -1.946166655054753614, 228.1230067974157691, 6.594641503551242678 ) ) ;
#5475 = CYLINDRICAL_SURFACE ( 'NONE', #3217, 1.000000000000000888 ) ;
#5476 = CARTESIAN_POINT ( 'NONE',  ( -5.375605342016473998, 2.665598297262353533, 18.50312048902377526 ) ) ;
#5477 = CARTESIAN_POINT ( 'NONE',  ( -2.066987299999999195, -0.8561741729129467293, -0.2999999989075252671 ) ) ;
#5478 = CARTESIAN_POINT ( 'NONE',  ( -2.500000000000000888, 188.4500000000000171, 8.035533905932737753 ) ) ;
#5479 = FACE_BOUND ( 'NONE', #6730, .T. ) ;
#5480 = EDGE_CURVE ( 'NONE', #2929, #9483, #686, .T. ) ;
#5482 = ORIENTED_EDGE ( 'NONE', *, *, #12795, .F. ) ;
#5481 = CARTESIAN_POINT ( 'NONE',  ( -6.403569081242510563E-16, 188.2499999989075263, 9.066987300000000971 ) ) ;
#5483 = CARTESIAN_POINT ( 'NONE',  ( -3.011139120916564327, -5.190534000030312178, 17.20068193741824558 ) ) ;
#5484 = MECHANICAL_DESIGN_GEOMETRIC_PRESENTATION_REPRESENTATION (  '', ( #7001 ), #2931 ) ;
#5485 = LINE ( 'NONE', #3449, #14411 ) ;
#5486 = CARTESIAN_POINT ( 'NONE',  ( -7.799024015210657801, -1.482594289697236389, 31.00000000000000000 ) ) ;
#5487 = CARTESIAN_POINT ( 'NONE',  ( 2.199649899629913641, 189.3965398499018136, 4.963263318916532718 ) ) ;
#5488 = CARTESIAN_POINT ( 'NONE',  ( 2.030576276931546336E-13, -6.250000000000000888, 25.49999999999999645 ) ) ;
#5489 = CARTESIAN_POINT ( 'NONE',  ( -0.1306497350717108763, 6.000000000000002665, 30.00000000000000711 ) ) ;
#5490 = CARTESIAN_POINT ( 'NONE',  ( 1.785787022451674089, 228.5490719641819908, 7.825142006337427070 ) ) ;
#5491 = CARTESIAN_POINT ( 'NONE',  ( 6.106056299406789734, -1.336851112280482035, 23.70112161576661336 ) ) ;
#5492 = CARTESIAN_POINT ( 'NONE',  ( -5.317509234263969375, 2.779225709350973350, 5.000000000000004441 ) ) ;
#5493 = DIRECTION ( 'NONE',  ( 0.000000000000000000, 0.000000000000000000, -1.000000000000000000 ) ) ;
#5494 = ORIENTED_EDGE ( 'NONE', *, *, #9992, .T. ) ;
#5495 = CARTESIAN_POINT ( 'NONE',  ( 1.461580736456472795, 185.7499999989074979, 8.461580736456474128 ) ) ;
#5496 = CARTESIAN_POINT ( 'NONE',  ( -0.9999502950801375523, 5.916088184763895086, 11.63108149190012064 ) ) ;
#5497 = EDGE_CURVE ( 'NONE', #11100, #9629, #10636, .T. ) ;
#5498 = EDGE_LOOP ( 'NONE', ( #2266, #6543, #11700, #12194 ) ) ;
#5499 = CYLINDRICAL_SURFACE ( 'NONE', #5066, 1.000000000000000888 ) ;
#5500 = CARTESIAN_POINT ( 'NONE',  ( 1.767766952966369320, 185.7000000000000171, 5.232233047033630235 ) ) ;
#5501 = CARTESIAN_POINT ( 'NONE',  ( -5.866923913994636308, -1.260079467906572770, 30.20047945897284336 ) ) ;
#5502 = CARTESIAN_POINT ( 'NONE',  ( -0.5044069930201934282, 5.979990686695005664, 18.87335743227902896 ) ) ;
#5503 =( NAMED_UNIT ( * ) PLANE_ANGLE_UNIT ( ) SI_UNIT ( $, .RADIAN. ) );
#5504 = CARTESIAN_POINT ( 'NONE',  ( -3.781065399485917133, -4.978303713186513768, 5.999917418102895361 ) ) ;
#5505 = CARTESIAN_POINT ( 'NONE',  ( 2.500000000000000000, 3.061616997868383141E-16, -1.900000000000000133 ) ) ;
#5506 = DIRECTION ( 'NONE',  ( 0.000000000000000000, -1.000000000000000000, 0.000000000000000000 ) ) ;
#5507 = CARTESIAN_POINT ( 'NONE',  ( 5.999999999999999112, 202.3202208672780102, 7.308763624231163547 ) ) ;
#5508 = DIRECTION ( 'NONE',  ( -0.9510565162951545304, 0.3090169943749447867, 0.000000000000000000 ) ) ;
#5509 = CARTESIAN_POINT ( 'NONE',  ( -5.665308849928776702, -1.980336949702643512, 17.00007997643737312 ) ) ;
#5510 = CARTESIAN_POINT ( 'NONE',  ( -13.50000000000000000, 2.000000000000000000, -1.999999999999997113 ) ) ;
#5511 = ORIENTED_EDGE ( 'NONE', *, *, #7181, .F. ) ;
#5512 = ORIENTED_EDGE ( 'NONE', *, *, #5166, .T. ) ;
#5513 = EDGE_LOOP ( 'NONE', ( #13468, #13148 ) ) ;
#5514 = CARTESIAN_POINT ( 'NONE',  ( 3.106366801611900819, -5.134708448381346102, 25.37303779027051576 ) ) ;
#5515 = DIRECTION ( 'NONE',  ( -0.9510565162951544194, 0.3090169943749447312, 0.000000000000000000 ) ) ;
#5516 = VERTEX_POINT ( 'NONE', #15414 ) ;
#5517 = PRODUCT_DEFINITION_SHAPE ( 'NONE', 'NONE',  #15739 ) ;
#5518 = CARTESIAN_POINT ( 'NONE',  ( 2.500000000000000444, 1.035533905932737975, 0.6500000021849496878 ) ) ;
#5519 = EDGE_CURVE ( 'NONE', #6636, #8784, #2571, .T. ) ;
#5520 = CARTESIAN_POINT ( 'NONE',  ( -2.931156713028478134, 5.520271803279214851, 31.50436969680152899 ) ) ;
#5521 = CYLINDRICAL_SURFACE ( 'NONE', #7469, 1.499999999999999556 ) ;
#5522 = CARTESIAN_POINT ( 'NONE',  ( -4.438452643612533777E-16, 185.0499999989075093, 9.066987300000000971 ) ) ;
#5523 = CARTESIAN_POINT ( 'NONE',  ( -1.530808498934191571E-16, 2.500000000000000000, 2.306999999978150306 ) ) ;
#5524 = EDGE_CURVE ( 'NONE', #8289, #6892, #9619, .T. ) ;
#5525 = CARTESIAN_POINT ( 'NONE',  ( -5.131373506000731055, 7.062729720844018289, 31.00000000000000000 ) ) ;
#5526 = CARTESIAN_POINT ( 'NONE',  ( -1.461580736456472795, 1.461580736456472795, 0.3500000010924746996 ) ) ;
#5527 = CARTESIAN_POINT ( 'NONE',  ( 1.035533905932737753, 188.9199999975965341, 4.500000000000000888 ) ) ;
#5528 = CARTESIAN_POINT ( 'NONE',  ( 1.707343418157801551, 228.0835877007203294, 9.663887492166837845 ) ) ;
#5529 = EDGE_CURVE ( 'NONE', #12097, #320, #14529, .T. ) ;
#5530 = LINE ( 'NONE', #14028, #7742 ) ;
#5531 = VERTEX_POINT ( 'NONE', #2356 ) ;
#5532 = CARTESIAN_POINT ( 'NONE',  ( 2.483278259701947821, -0.3214162717929257562, -2.499187116769100658 ) ) ;
#5533 = B_SPLINE_CURVE_WITH_KNOTS ( 'NONE', 3,
 ( #14440, #13009, #10631, #8250, #8414, #3621, #9766, #8328, #14522, #7055, #12055, #3543, #9683, #6104, #15567, #4747, #5785, #2347 ),
 .UNSPECIFIED., .F., .F.,
 ( 4, 2, 2, 2, 2, 2, 2, 2, 4 ),
 ( 0.003131918686235970421, 0.003523310662250261124, 0.003914702638264551393, 0.004306094614278842096, 0.004697486590293132799, 0.005088878566307422635, 0.005480270542321714206, 0.005871662518336004041, 0.006263054494350294744 ),
 .UNSPECIFIED. ) ;
#5534 = VERTEX_POINT ( 'NONE', #3469 ) ;
#5535 = LINE ( 'NONE', #14337, #8364 ) ;
#5536 = VECTOR ( 'NONE', #15673, 1000.000000000000000 ) ;
#5537 = CARTESIAN_POINT ( 'NONE',  ( 2.094888806938587637E-14, 6.250000000000000888, 30.00000000000000000 ) ) ;
#5538 = CARTESIAN_POINT ( 'NONE',  ( -0.2622916576876674899, 5.995491482261829042, 5.973849426468138546 ) ) ;
#5539 = ORIENTED_EDGE ( 'NONE', *, *, #3553, .T. ) ;
#5540 = DIRECTION ( 'NONE',  ( 0.9510565162951499785, 0.3090169943749582204, 0.000000000000000000 ) ) ;
#5541 = CARTESIAN_POINT ( 'NONE',  ( 1.767766984964215471, 1.767766920968521616, -2.500000000000000444 ) ) ;
#5542 = DIRECTION ( 'NONE',  ( 0.000000000000000000, -1.000000000000000000, 0.000000000000000000 ) ) ;
#5543 = CARTESIAN_POINT ( 'NONE',  ( -1.035533905932738197, -2.500000000000000000, -1.350000000000000089 ) ) ;
#5544 = CARTESIAN_POINT ( 'NONE',  ( -4.322356511625788045, 7.650514973136498753, 31.00000000000000000 ) ) ;
#5545 = SURFACE_STYLE_USAGE ( .BOTH. , #15487 ) ;
#5546 = CIRCLE ( 'NONE', #211, 1.499999999999999556 ) ;
#5547 = CARTESIAN_POINT ( 'NONE',  ( 0.0008067760839495599114, 0.4000000000000062395, -2.465784186028391112 ) ) ;
#5548 = CARTESIAN_POINT ( 'NONE',  ( 1.035533905932737975, 185.6499999978150868, 4.500000000000000888 ) ) ;
#5549 = AXIS2_PLACEMENT_3D ( 'NONE', #3033, #14001, #633 ) ;
#5550 = CARTESIAN_POINT ( 'NONE',  ( 0.8239120926223584274, 228.2181226988968774, 10.05946334177977519 ) ) ;
#5551 = DIRECTION ( 'NONE',  ( 0.000000000000000000, 0.000000000000000000, -1.000000000000000000 ) ) ;
#5552 = CARTESIAN_POINT ( 'NONE',  ( 0.8730628416139659675, 6.188929913094928459, 23.99504929893123517 ) ) ;
#5553 = CARTESIAN_POINT ( 'NONE',  ( 3.796994071234844259E-16, -2.066987299999999639, -1.749999998907525223 ) ) ;
#5554 = CARTESIAN_POINT ( 'NONE',  ( 2.500000000000000444, 186.3499999999999943, 8.035533905932739529 ) ) ;
#5555 = CARTESIAN_POINT ( 'NONE',  ( -4.416837305303647376, 4.422286678978860408, 24.76190213084012726 ) ) ;
#5556 = CIRCLE ( 'NONE', #15202, 1.999999999999999556 ) ;
#5558 = ORIENTED_EDGE ( 'NONE', *, *, #5221, .T. ) ;
#5557 = FACE_OUTER_BOUND ( 'NONE', #13867, .T. ) ;
#5559 = ADVANCED_FACE ( 'NONE', ( #1241 ), #14449, .F. ) ;
#5560 = DIRECTION ( 'NONE',  ( -6.123233995736766036E-17, 1.000000000000000000, 0.000000000000000000 ) ) ;
#5561 = CARTESIAN_POINT ( 'NONE',  ( -5.866984344570817633, 1.259800266528702917, 23.70068193741825269 ) ) ;
#5562 = CARTESIAN_POINT ( 'NONE',  ( -1.342063929050375748, 190.0567506639880833, 4.518418250680232617 ) ) ;
#5563 = CARTESIAN_POINT ( 'NONE',  ( 5.317509234263979145, -2.779225709350955142, 31.00000000000000000 ) ) ;
#5564 = ADVANCED_FACE ( 'NONE', ( #2437 ), #13258, .T. ) ;
#5565 = LINE ( 'NONE', #3634, #8768 ) ;
#5566 = CARTESIAN_POINT ( 'NONE',  ( 2.500000000000000444, 185.5800000002185186, 5.964466094067262247 ) ) ;
#5567 = CARTESIAN_POINT ( 'NONE',  ( -5.903119516422476565, -1.077859910107483943, 5.615193824488508234 ) ) ;
#5568 = CARTESIAN_POINT ( 'NONE',  ( 1.990705347729657237, 228.2501094229765215, 6.961721135629644230 ) ) ;
#5569 = DIRECTION ( 'NONE',  ( -0.3090169943749447867, -0.9510565162951544194, 0.000000000000000000 ) ) ;
#5570 = CARTESIAN_POINT ( 'NONE',  ( 0.06795095462586417390, 0.4000000000000045186, 2.547546041960362828 ) ) ;
#5571 = DIRECTION ( 'NONE',  ( 1.062480551894331009E-17, -2.775557561562888393E-16, 1.000000000000000000 ) ) ;
#5572 = ORIENTED_EDGE ( 'NONE', *, *, #6976, .T. ) ;
#5573 = CARTESIAN_POINT ( 'NONE',  ( 0.8561741729129457301, 189.0999999989075206, 9.066987299999999195 ) ) ;
#5574 = CARTESIAN_POINT ( 'NONE',  ( -0.6152055445545627776, 5.969096820685162896, 12.29904968670266108 ) ) ;
#5575 = VERTEX_POINT ( 'NONE', #7376 ) ;
#5576 = DIRECTION ( 'NONE',  ( -0.3090169943749579429, 0.9510565162951502005, 0.000000000000000000 ) ) ;
#5577 = CARTESIAN_POINT ( 'NONE',  ( 5.131373506000584506, 7.062729720844102665, 31.00000000000000000 ) ) ;
#5578 = B_SPLINE_CURVE_WITH_KNOTS ( 'NONE', 3,
 ( #12987, #2985, #12914, #1936, #2015, #6810, #513, #7836, #6656, #11645, #6888, #5382, #6733, #825, #7911, #15080, #1781, #11487 ),
 .UNSPECIFIED., .F., .F.,
 ( 4, 2, 2, 2, 2, 2, 2, 2, 4 ),
 ( 0.003131486019301991160, 0.003522824630466697866, 0.003914163241631405006, 0.004305501852796111278, 0.004696840463960818418, 0.005088179075125525558, 0.005479517686290231830, 0.005870856297454938102, 0.006262194908619645242 ),
 .UNSPECIFIED. ) ;
#5579 = CARTESIAN_POINT ( 'NONE',  ( -5.375605342016489097, -2.665598297262326444, 30.49687951097621053 ) ) ;
#5580 = FACE_OUTER_BOUND ( 'NONE', #11484, .T. ) ;
#5581 = CARTESIAN_POINT ( 'NONE',  ( 5.935543223013866942, 0.8771126767606117758, 17.99999999999998934 ) ) ;
#5582 = LINE ( 'NONE', #9906, #2528 ) ;
#5583 = CARTESIAN_POINT ( 'NONE',  ( -3.159082487394711869, -5.393634094348371377, 5.799544624688432570 ) ) ;
#5584 = CARTESIAN_POINT ( 'NONE',  ( 1.035533905932737531, 2.500000000000000444, -0.9500000000000001776 ) ) ;
#5585 = CARTESIAN_POINT ( 'NONE',  ( 4.005998022989988527, -4.467726698309236077, 10.70068193741824913 ) ) ;
#5586 = FACE_OUTER_BOUND ( 'NONE', #9560, .T. ) ;
#5587 = CYLINDRICAL_SURFACE ( 'NONE', #6745, 1.000000000000000888 ) ;
#5588 = CARTESIAN_POINT ( 'NONE',  ( -1.265664690411614835E-16, 2.066987299999999639, -2.749999998907525001 ) ) ;
#5589 = CARTESIAN_POINT ( 'NONE',  ( -4.286401442266546624, -4.198423832313178394, 31.00000000000000000 ) ) ;
#5590 = VERTEX_POINT ( 'NONE', #1392 ) ;
#5591 = MECHANICAL_DESIGN_GEOMETRIC_PRESENTATION_REPRESENTATION (  '', ( #11677 ), #11178 ) ;
#5592 = ORIENTED_EDGE ( 'NONE', *, *, #10914, .T. ) ;
#5593 = ORIENTED_EDGE ( 'NONE', *, *, #677, .F. ) ;
#5594 = CARTESIAN_POINT ( 'NONE',  ( -6.081509788407728045, -1.446521464462759976, 10.62618035954927898 ) ) ;
#5595 = FACE_BOUND ( 'NONE', #8329, .T. ) ;
#5596 = EDGE_LOOP ( 'NONE', ( #3159, #9665, #5712 ) ) ;
#5597 = CARTESIAN_POINT ( 'NONE',  ( 5.317509234264033324, -2.779225709350851670, 18.13239388001634467 ) ) ;
#5598 = CARTESIAN_POINT ( 'NONE',  ( -2.500000000000000000, 0.000000000000000000, 0.2000000021849495657 ) ) ;
#5599 = CARTESIAN_POINT ( 'NONE',  ( -0.6152055445544284407, 5.969096820685177995, 25.29904968670266996 ) ) ;
#5600 = CARTESIAN_POINT ( 'NONE',  ( -3.567624405365222628, -5.133384272590791220, 4.000049210157070156 ) ) ;
#5601 = CARTESIAN_POINT ( 'NONE',  ( 3.726944967918921492E-17, 185.4499999989075150, 4.933012699999999029 ) ) ;
#5602 = CARTESIAN_POINT ( 'NONE',  ( -2.500000000000000444, 1.035533905932737753, 1.656999999978150617 ) ) ;
#5603 = DIRECTION ( 'NONE',  ( 0.8090169943749506709, -0.5877852522924686962, 0.000000000000000000 ) ) ;
#5604 = PRODUCT_CONTEXT ( 'NONE', #8631, 'mechanical' ) ;
#5605 = CARTESIAN_POINT ( 'NONE',  ( 1.461580736456473018, -1.461580736456472573, 0.7500000010924746663 ) ) ;
#5606 = CARTESIAN_POINT ( 'NONE',  ( -5.903057025253906964, -1.078199533779497177, 4.384382673013948128 ) ) ;
#5607 = CARTESIAN_POINT ( 'NONE',  ( -1.958673816210946272, 228.3772695101851014, 7.328966720224260101 ) ) ;
#5608 = CARTESIAN_POINT ( 'NONE',  ( 1.767766952966368654, 1.767766952966369098, 0.7000000021849498433 ) ) ;
#5609 = VERTEX_POINT ( 'NONE', #7225 ) ;
#5610 = CARTESIAN_POINT ( 'NONE',  ( 1.035533905932739085, -2.500000000000000000, 0.4500000021849498433 ) ) ;
#5611 = VERTEX_POINT ( 'NONE', #11105 ) ;
#5612 = EDGE_CURVE ( 'NONE', #3208, #5348, #6113, .T. ) ;
#5613 = CARTESIAN_POINT ( 'NONE',  ( -0.2619041840694215084, 6.245686665308503471, 10.52605849433793672 ) ) ;
#5614 = CARTESIAN_POINT ( 'NONE',  ( 2.500000000000000000, 189.4999999978150527, 7.000000000000000000 ) ) ;
#5615 = DIRECTION ( 'NONE',  ( 0.000000000000000000, 1.000000000000000000, 0.000000000000000000 ) ) ;
#5616 = ORIENTED_EDGE ( 'NONE', *, *, #11851, .T. ) ;
#5617 = CARTESIAN_POINT ( 'NONE',  ( 3.458623254138665448, 5.207221900902852418, 10.52622717124729945 ) ) ;
#5618 = EDGE_CURVE ( 'NONE', #10533, #12135, #7159, .T. ) ;
#5619 = FACE_BOUND ( 'NONE', #10787, .T. ) ;
#5620 = CARTESIAN_POINT ( 'NONE',  ( 4.069684453406282820, -4.744965295353568813, 17.12619944752603729 ) ) ;
#5621 = CARTESIAN_POINT ( 'NONE',  ( 2.500000000000000000, 3.061616997868383141E-16, -1.900000000000000133 ) ) ;
#5622 = CARTESIAN_POINT ( 'NONE',  ( 2.500000000000000444, 185.5999999999999943, 7.000000000000000000 ) ) ;
#5623 = FACE_OUTER_BOUND ( 'NONE', #3601, .T. ) ;
#5624 = CARTESIAN_POINT ( 'NONE',  ( 2.500000000000000444, 185.4499999978150981, 8.035533905932739529 ) ) ;
#5625 = ADVANCED_FACE ( 'NONE', ( #4834 ), #14614, .F. ) ;
#5626 = CARTESIAN_POINT ( 'NONE',  ( -1.691178964804313178, 228.6047289695326583, 7.985882612257780622 ) ) ;
#5627 = FACE_BOUND ( 'NONE', #10514, .T. ) ;
#5628 = CARTESIAN_POINT ( 'NONE',  ( -5.915641100987815371, 1.003868594704848238, 18.50428920362019269 ) ) ;
#5629 = ADVANCED_FACE ( 'NONE', ( #8335 ), #8505, .T. ) ;
#5630 = CARTESIAN_POINT ( 'NONE',  ( 1.461580736456473018, -1.461580736456472573, -2.449999998907525622 ) ) ;
#5631 = B_SPLINE_CURVE_WITH_KNOTS ( 'NONE', 3,
 ( #2620, #7476, #12320, #1415, #7549, #3729, #1342, #9869, #6452, #2698, #151, #8607, #12474, #11131, #14870, #6373, #4043, #2545 ),
 .UNSPECIFIED., .F., .F.,
 ( 4, 2, 2, 2, 2, 2, 2, 2, 4 ),
 ( 0.000000000000000000, 0.0003914898357794973868, 0.0007829796715589947735, 0.001174469507338492215, 0.001565959343117989547, 0.001957449178897487096, 0.002348939014676984429, 0.002740428850456481762, 0.003131918686235979094 ),
 .UNSPECIFIED. ) ;
#5632 = CARTESIAN_POINT ( 'NONE',  ( -6.776263578034402713E-18, 186.5999999999999943, 4.500000000000000000 ) ) ;
#5633 = CARTESIAN_POINT ( 'NONE',  ( -4.152999119458150368, 4.671604476854199106, 25.30026515017674171 ) ) ;
#5635 = VERTEX_POINT ( 'NONE', #6029 ) ;
#5634 = CARTESIAN_POINT ( 'NONE',  ( -0.9739805876845880617, -5.920636045238200751, 24.76171386814422704 ) ) ;
#5636 = CARTESIAN_POINT ( 'NONE',  ( -5.558508435838166228, 2.857531096718976649, 17.99999999999998934 ) ) ;
#5637 = CARTESIAN_POINT ( 'NONE',  ( -2.727823417914460258, 189.8175560065074023, 8.604987984268861467 ) ) ;
#5638 = DIRECTION ( 'NONE',  ( 0.5877852522924802425, -0.8090169943749422332, 0.000000000000000000 ) ) ;
#5639 = CARTESIAN_POINT ( 'NONE',  ( 2.500000000000000444, 183.9800000002184959, 5.964466094067262247 ) ) ;
#5640 = CARTESIAN_POINT ( 'NONE',  ( 2.082642335314403343E-14, 6.000000000000000888, 32.00000000000000000 ) ) ;
#5641 = CARTESIAN_POINT ( 'NONE',  ( 1.360905158423219241, 228.7363411735375962, 8.365986164091459898 ) ) ;
#5642 = CARTESIAN_POINT ( 'NONE',  ( 0.000000000000000000, 0.000000000000000000, 2.500000000000000000 ) ) ;
#5643 = CARTESIAN_POINT ( 'NONE',  ( 0.000000000000000000, 0.4000000000000097367, 2.450963827680236129 ) ) ;
#5644 = VECTOR ( 'NONE', #4379, 1000.000000000000114 ) ;
#5645 = CARTESIAN_POINT ( 'NONE',  ( -1.767766952966368432, -1.767766952966369320, 1.100000002184950088 ) ) ;
#5646 = ORIENTED_EDGE ( 'NONE', *, *, #9307, .F. ) ;
#5647 = CARTESIAN_POINT ( 'NONE',  ( -0.8561741729129457301, 185.2999999989075377, 4.933012699999999029 ) ) ;
#5648 = CARTESIAN_POINT ( 'NONE',  ( 7.180990026460803755, -3.384707322287205944, 24.49999999999999289 ) ) ;
#5649 = ORIENTED_EDGE ( 'NONE', *, *, #11273, .F. ) ;
#5650 = EDGE_CURVE ( 'NONE', #10770, #8478, #13008, .T. ) ;
#5651 = DIRECTION ( 'NONE',  ( -0.5877852522924685852, -0.8090169943749508930, 0.000000000000000000 ) ) ;
#5652 = PRODUCT_RELATED_PRODUCT_CATEGORY ( 'part', '', ( #7157 ) ) ;
#5653 = AXIS2_PLACEMENT_3D ( 'NONE', #13457, #11941, #7417 ) ;
#5655 = B_SPLINE_CURVE_WITH_KNOTS ( 'NONE', 3,
 ( #1266, #1345, #14558, #13445, #8686, #3654, #10979, #7402, #12245, #11055, #154, #14873, #15032, #12477, #12399, #6293, #7707, #4126 ),
 .UNSPECIFIED., .F., .F.,
 ( 4, 2, 2, 2, 2, 2, 2, 2, 4 ),
 ( 0.003131918686235975625, 0.003523310662250265894, 0.003914702638264555730, 0.004306094614278846433, 0.004697486590293136269, 0.005088878566307426105, 0.005480270542321715940, 0.005871662518336005776, 0.006263054494350296479 ),
 .UNSPECIFIED. ) ;
#5654 = CARTESIAN_POINT ( 'NONE',  ( 2.500000000000000000, 3.061616997868383141E-16, 2.500000000000000000 ) ) ;
#5656 = ADVANCED_FACE ( 'NONE', ( #13801 ), #2754, .F. ) ;
#5657 = CARTESIAN_POINT ( 'NONE',  ( 5.903347812666365435, 1.076697810262510213, 17.38602261056917087 ) ) ;
#5658 = CARTESIAN_POINT ( 'NONE',  ( 2.066987300000000527, 187.4499999989075150, 7.000000000000000000 ) ) ;
#5659 = DIRECTION ( 'NONE',  ( 0.000000000000000000, 1.000000000000000000, 0.000000000000000000 ) ) ;
#5660 = CARTESIAN_POINT ( 'NONE',  ( 1.767766952966368654, 1.767766952966369098, -0.8999999978150502455 ) ) ;
#5661 = DIRECTION ( 'NONE',  ( 0.000000000000000000, 0.000000000000000000, 1.000000000000000000 ) ) ;
#5662 = CARTESIAN_POINT ( 'NONE',  ( 3.659182332138577465E-16, 189.3270225533669020, 3.938484906660876472 ) ) ;
#5663 = DIRECTION ( 'NONE',  ( 0.000000000000000000, 0.000000000000000000, 1.000000000000000000 ) ) ;
#5664 = CARTESIAN_POINT ( 'NONE',  ( 4.435347140100995844, 4.403429997944549257, 31.00000000000000000 ) ) ;
#5665 = CARTESIAN_POINT ( 'NONE',  ( 5.935543223013857173, 0.8771126767606810537, 11.63061695532135609 ) ) ;
#5666 = VERTEX_POINT ( 'NONE', #12531 ) ;
#5667 = AXIS2_PLACEMENT_3D ( 'NONE', #5856, #4423, #9590 ) ;
#5668 = ORIENTED_EDGE ( 'NONE', *, *, #9950, .F. ) ;
#5669 = ORIENTED_EDGE ( 'NONE', *, *, #3765, .F. ) ;
#5670 = CARTESIAN_POINT ( 'NONE',  ( 4.005785023174367687, -4.467917056767481299, 25.29952054102715309 ) ) ;
#5671 = FACE_OUTER_BOUND ( 'NONE', #10985, .T. ) ;
#5672 = VERTEX_POINT ( 'NONE', #2911 ) ;
#5673 = CARTESIAN_POINT ( 'NONE',  ( 5.866817325727538446, -1.260653813891827291, 18.80022217383877958 ) ) ;
#5674 = CARTESIAN_POINT ( 'NONE',  ( 2.500000000000000000, 3.061616997868383141E-16, -0.9999999978150503344 ) ) ;
#5675 = CARTESIAN_POINT ( 'NONE',  ( 7.347880794884119736E-16, -6.250000000000000888, 4.000000000000004441 ) ) ;
#5676 = CARTESIAN_POINT ( 'NONE',  ( 0.000000000000000000, 0.000000000000000000, 2.000000000000001776 ) ) ;
#5677 = CARTESIAN_POINT ( 'NONE',  ( -1.767766952966369320, 188.9999999978150527, 5.232233047033630235 ) ) ;
#5678 = AXIS2_PLACEMENT_3D ( 'NONE', #4545, #8047, #799 ) ;
#5679 = CARTESIAN_POINT ( 'NONE',  ( 2.500000000000000444, 1.035533905932737975, -1.043000000021849560 ) ) ;
#5680 = CYLINDRICAL_SURFACE ( 'NONE', #7694, 0.9999999999999998890 ) ;
#5681 = APPLICATION_PROTOCOL_DEFINITION ( 'draft international standard', 'automotive_design', 1998, #477 ) ;
#5682 = FACE_OUTER_BOUND ( 'NONE', #15685, .T. ) ;
#5683 = CARTESIAN_POINT ( 'NONE',  ( -7.180990026460705167, -3.384707322287646480, 17.99999999999998934 ) ) ;
#5684 = CARTESIAN_POINT ( 'NONE',  ( 0.7798766585422360897, 226.3581810736479270, 4.583957619654694504 ) ) ;
#5685 = CARTESIAN_POINT ( 'NONE',  ( -0.7777163206635004933, 228.2226383035325057, 10.07273956871427956 ) ) ;
#5686 = ORIENTED_EDGE ( 'NONE', *, *, #10963, .T. ) ;
#5687 = CARTESIAN_POINT ( 'NONE',  ( -1.880234698852980557, -1.653780175538818620, -2.499419789153938698 ) ) ;
#5688 = AXIS2_PLACEMENT_3D ( 'NONE', #8361, #8442, #6053 ) ;
#5689 = VERTEX_POINT ( 'NONE', #7761 ) ;
#5690 = CARTESIAN_POINT ( 'NONE',  ( 2.841163418881473834, -5.567120626447887410, 5.262369734438755664 ) ) ;
#5691 = ADVANCED_FACE ( 'NONE', ( #1705 ), #6581, .F. ) ;
#5692 = CARTESIAN_POINT ( 'NONE',  ( 7.490007020835706797, -2.433650805992179755, 11.49999999999998224 ) ) ;
#5693 = PRODUCT_RELATED_PRODUCT_CATEGORY ( 'part', '', ( #4768 ) ) ;
#5694 = CARTESIAN_POINT ( 'NONE',  ( -0.6139908388541001072, 5.969238533166612015, 4.199776279120134070 ) ) ;
#5695 = ORIENTED_EDGE ( 'NONE', *, *, #534, .F. ) ;
#5696 = CARTESIAN_POINT ( 'NONE',  ( 3.566234721238037864, 5.134387337253831340, 10.50008258189709132 ) ) ;
#5697 = FACE_BOUND ( 'NONE', #498, .T. ) ;
#5698 = CARTESIAN_POINT ( 'NONE',  ( -2.500000000000000000, 0.000000000000000000, 1.700000000000000178 ) ) ;
#5699 = CARTESIAN_POINT ( 'NONE',  ( 4.592425496802573972E-16, -2.500000000000000000, -1.300000000000000044 ) ) ;
#5700 = CARTESIAN_POINT ( 'NONE',  ( 0.000000000000000000, 2.000000000000000000, 0.000000000000000000 ) ) ;
#5701 = CARTESIAN_POINT ( 'NONE',  ( -2.500000000000000000, 0.000000000000000000, 1.800000002184949821 ) ) ;
#5702 = CARTESIAN_POINT ( 'NONE',  ( -1.767766952966369765, 188.5000000000000000, 8.767766952966368876 ) ) ;
#5703 = EDGE_CURVE ( 'NONE', #9607, #1897, #4420, .T. ) ;
#5704 = CARTESIAN_POINT ( 'NONE',  ( -1.965306002007385144, 228.1545512627131131, 6.685743718507844768 ) ) ;
#5705 = FACE_BOUND ( 'NONE', #7483, .T. ) ;
#5706 = LINE ( 'NONE', #10550, #6209 ) ;
#5707 = AXIS2_PLACEMENT_3D ( 'NONE', #12298, #54, #9776 ) ;
#5708 = CARTESIAN_POINT ( 'NONE',  ( 0.01194215579347689300, 189.0000000000000568, 4.500000000000001776 ) ) ;
#5709 = CARTESIAN_POINT ( 'NONE',  ( 1.035533905932737753, 188.1499999999999773, 4.500000000000000888 ) ) ;
#5710 = CYLINDRICAL_SURFACE ( 'NONE', #7077, 1.000000000000000888 ) ;
#5712 = ORIENTED_EDGE ( 'NONE', *, *, #8880, .F. ) ;
#5711 = DIRECTION ( 'NONE',  ( 0.8090169943749506709, -0.5877852522924689183, 0.000000000000000000 ) ) ;
#5713 = CARTESIAN_POINT ( 'NONE',  ( -5.858813228503629844, 2.179803269293333123, 18.97377282875267213 ) ) ;
#5714 = ORIENTED_EDGE ( 'NONE', *, *, #3943, .T. ) ;
#5715 = VECTOR ( 'NONE', #7872, 1000.000000000000114 ) ;
#5716 = FACE_OUTER_BOUND ( 'NONE', #3442, .T. ) ;
#5717 = CARTESIAN_POINT ( 'NONE',  ( -1.974820130016563091, 226.5603787955025155, 5.179955460749784635 ) ) ;
#5718 = ADVANCED_FACE ( 'NONE', ( #9127 ), #15238, .F. ) ;
#5719 = CARTESIAN_POINT ( 'NONE',  ( 1.442725981297484195, 190.0517701937062043, 4.572028445994527956 ) ) ;
#5720 = CARTESIAN_POINT ( 'NONE',  ( -2.500000000000000444, 184.2800000002184504, 5.964466094067261359 ) ) ;
#5721 = CARTESIAN_POINT ( 'NONE',  ( -0.6152055445546077417, 5.969096820685158455, 31.79904968670268417 ) ) ;
#5722 = EDGE_CURVE ( 'NONE', #6460, #5344, #6815, .T. ) ;
#5723 = CARTESIAN_POINT ( 'NONE',  ( 1.312858199469658427, 228.7505821040874139, 8.407114783769989330 ) ) ;
#5724 = FACE_BOUND ( 'NONE', #2244, .T. ) ;
#5725 = CARTESIAN_POINT ( 'NONE',  ( -5.615973259022345232, 2.743340227996120539, 4.496107868750329750 ) ) ;
#5726 = DIRECTION ( 'NONE',  ( -1.000000000000000000, 0.000000000000000000, 0.000000000000000000 ) ) ;
#5727 = ORIENTED_EDGE ( 'NONE', *, *, #7781, .T. ) ;
#5728 = CARTESIAN_POINT ( 'NONE',  ( -1.461580736456473684, 185.5499999989075093, 8.461580736456474128 ) ) ;
#5729 = CARTESIAN_POINT ( 'NONE',  ( 4.195795028115036018, 4.289273350251318284, 30.49571079637980020 ) ) ;
#5730 = ORIENTED_EDGE ( 'NONE', *, *, #6320, .F. ) ;
#5731 = CARTESIAN_POINT ( 'NONE',  ( 2.500000000000000444, 184.0000000000000000, 7.000000000000000000 ) ) ;
#5732 = CARTESIAN_POINT ( 'NONE',  ( -2.668367453516726773, 5.373994336898084256, 31.13239388001635177 ) ) ;
#5733 = CARTESIAN_POINT ( 'NONE',  ( 2.996920846510391812, 5.485395142346844111, 17.38558052754515160 ) ) ;
#5734 = CARTESIAN_POINT ( 'NONE',  ( -1.461580736456473240, 187.7499999989075263, 5.538419263543526760 ) ) ;
#5735 = CARTESIAN_POINT ( 'NONE',  ( -1.000049271338272705, 6.169473353325585663, 24.36969612704542243 ) ) ;
#5736 = CARTESIAN_POINT ( 'NONE',  ( -1.035533905932737753, 2.500000000000000444, 0.05000000218494983495 ) ) ;
#5737 = CARTESIAN_POINT ( 'NONE',  ( 3.312524433819828307, -5.004191858253970615, 10.52591947216897772 ) ) ;
#5738 = AXIS2_PLACEMENT_3D ( 'NONE', #8418, #4913, #7447 ) ;
#5739 = CARTESIAN_POINT ( 'NONE',  ( 3.659182332138577465E-16, 188.6555110544239824, 3.692234042172417574 ) ) ;
#5740 = CIRCLE ( 'NONE', #131, 6.250000000000000888 ) ;
#5741 = CARTESIAN_POINT ( 'NONE',  ( 2.500000000000000000, 188.6999999978150697, 7.000000000000000000 ) ) ;
#5742 = CARTESIAN_POINT ( 'NONE',  ( -5.486741141153726353, -2.429871531109881300, 17.20111757752057002 ) ) ;
#5743 = EDGE_CURVE ( 'NONE', #12482, #12866, #4478, .T. ) ;
#5744 = FACE_OUTER_BOUND ( 'NONE', #4074, .T. ) ;
#5745 = ORIENTED_EDGE ( 'NONE', *, *, #3658, .T. ) ;
#5746 = VERTEX_POINT ( 'NONE', #5772 ) ;
#5747 = ORIENTED_EDGE ( 'NONE', *, *, #8942, .T. ) ;
#5748 = CARTESIAN_POINT ( 'NONE',  ( 2.817313151351090728, 5.579000502529481764, 30.86939309276503351 ) ) ;
#5749 = CARTESIAN_POINT ( 'NONE',  ( -3.632151824461123724, 4.777505256984569293, 12.50004932073310471 ) ) ;
#5750 = ORIENTED_EDGE ( 'NONE', *, *, #8030, .F. ) ;
#5751 = CARTESIAN_POINT ( 'NONE',  ( 1.035533905932737531, 2.500000000000000444, -0.8499999978150503122 ) ) ;
#5752 = CARTESIAN_POINT ( 'NONE',  ( 0.5039079366032432894, -5.980031194523151683, 4.126370681098135762 ) ) ;
#5753 = CARTESIAN_POINT ( 'NONE',  ( -2.841041022017302797, -5.567186575787308023, 4.737747182782873878 ) ) ;
#5754 = CARTESIAN_POINT ( 'NONE',  ( 2.500000000000000444, 187.8999999978150584, 7.000000000000000000 ) ) ;
#5755 = CARTESIAN_POINT ( 'NONE',  ( 2.500000000000000444, -1.035533905932737309, 0.4569999999781503286 ) ) ;
#5756 = CARTESIAN_POINT ( 'NONE',  ( -1.767766952966369098, 185.7999999978150356, 5.232233047033630235 ) ) ;
#5757 = APPLICATION_PROTOCOL_DEFINITION ( 'draft international standard', 'automotive_design', 1998, #8631 ) ;
#5758 = CARTESIAN_POINT ( 'NONE',  ( -1.461580736456472351, -1.461580736456473018, 1.350000001092474644 ) ) ;
#5759 = ADVANCED_FACE ( 'NONE', ( #2172 ), #4259, .T. ) ;
#5760 = B_SPLINE_CURVE_WITH_KNOTS ( 'NONE', 3,
 ( #8759, #14874, #2549, #3886, #12171, #6294, #3813, #312, #2384, #5098, #79, #10905, #12324, #9949, #14801, #14646, #9723, #4865 ),
 .UNSPECIFIED., .F., .F.,
 ( 4, 2, 2, 2, 2, 2, 2, 2, 4 ),
 ( 0.003131490185286092253, 0.003522829482338693183, 0.003914168779391293679, 0.004305508076443895042, 0.004696847373496496406, 0.005088186670549096902, 0.005479525967601697398, 0.005870865264654297894, 0.006262204561706899257 ),
 .UNSPECIFIED. ) ;
#5761 = CARTESIAN_POINT ( 'NONE',  ( -1.035533905932737975, 189.0199999975965568, 4.500000000000000888 ) ) ;
#5762 = CARTESIAN_POINT ( 'NONE',  ( 0.09803033623910094307, 226.3251703050289336, 4.486637493502143137 ) ) ;
#5763 = AXIS2_PLACEMENT_3D ( 'NONE', #9000, #13828, #2941 ) ;
#5764 = CARTESIAN_POINT ( 'NONE',  ( -0.09789622041826565035, 228.2551366570249343, 10.16828389758070550 ) ) ;
#5765 = VERTEX_POINT ( 'NONE', #6893 ) ;
#5766 = CARTESIAN_POINT ( 'NONE',  ( 2.848235266351075268, -5.281699484015620172, 4.386022610569179747 ) ) ;
#5767 = EDGE_LOOP ( 'NONE', ( #1742, #11702 ) ) ;
#5768 = DIRECTION ( 'NONE',  ( -1.000000000000000000, 3.326610055774637112E-18, 1.062480551894331163E-17 ) ) ;
#5769 = DIRECTION ( 'NONE',  ( -0.3090169943749446202, -0.9510565162951544194, 0.000000000000000000 ) ) ;
#5770 = FACE_BOUND ( 'NONE', #6870, .T. ) ;
#5771 = ORIENTED_EDGE ( 'NONE', *, *, #6124, .F. ) ;
#5772 = CARTESIAN_POINT ( 'NONE',  ( -5.935543223013841185, 0.8771126767608004027, 17.99999999999998934 ) ) ;
#5773 = CARTESIAN_POINT ( 'NONE',  ( 3.312524433819643122, 5.004191858254092296, 25.47408052783099919 ) ) ;
#5774 = FACE_BOUND ( 'NONE', #14628, .T. ) ;
#5775 = CARTESIAN_POINT ( 'NONE',  ( -2.997753866155852265, -5.484939622623827837, 18.61560192892920895 ) ) ;
#5776 = CARTESIAN_POINT ( 'NONE',  ( -2.500000000000000444, 1.035533905932737753, 0.8500000000000001998 ) ) ;
#5777 = CARTESIAN_POINT ( 'NONE',  ( -3.000000000000000444, -1.732050807568878081, -5.500000000000000000 ) ) ;
#5778 = CYLINDRICAL_SURFACE ( 'NONE', #11786, 0.9999999999999998890 ) ;
#5779 = PRODUCT_DEFINITION_SHAPE ( 'NONE', 'NONE',  #15754 ) ;
#5780 = CARTESIAN_POINT ( 'NONE',  ( -1.767766952966369542, 185.1999999978150697, 8.767766952966368876 ) ) ;
#5781 = CARTESIAN_POINT ( 'NONE',  ( -1.864336199031810581, 228.4898043637318779, 7.653973795834509097 ) ) ;
#5782 = B_SPLINE_CURVE_WITH_KNOTS ( 'NONE', 3,
 ( #5664, #7966, #14004, #637, #10511, #15366, #14157, #3260, #2066, #3036, #10354, #3112, #7014, #6939, #4307, #7889, #874, #954 ),
 .UNSPECIFIED., .F., .F.,
 ( 4, 2, 2, 2, 2, 2, 2, 2, 4 ),
 ( 0.000000000000000000, 0.0003914357524127466182, 0.0007828715048254932364, 0.001174307257238239909, 0.001565743009650987557, 0.001957178762063734988, 0.002348614514476482420, 0.002740050266889230285, 0.003131486019301977716 ),
 .UNSPECIFIED. ) ;
#5783 = CARTESIAN_POINT ( 'NONE',  ( 3.922288969639774248, 4.542045818322530515, 31.87378430870261425 ) ) ;
#5784 = VECTOR ( 'NONE', #12957, 1000.000000000000000 ) ;
#5785 = CARTESIAN_POINT ( 'NONE',  ( 5.317509234263941842, 2.779225709351030638, 31.13236078583911493 ) ) ;
#5786 = CARTESIAN_POINT ( 'NONE',  ( 1.035533905932738197, 188.6499999999999773, 9.500000000000003553 ) ) ;
#5787 = CARTESIAN_POINT ( 'NONE',  ( 5.935543223013856284, 0.8771126767606806096, 11.49999999999998224 ) ) ;
#5789 = ORIENTED_EDGE ( 'NONE', *, *, #3262, .F. ) ;
#5788 = CARTESIAN_POINT ( 'NONE',  ( 4.000000000000001776, 184.0000000000000000, 7.000000000000000000 ) ) ;
#5790 = CYLINDRICAL_SURFACE ( 'NONE', #7406, 1.000000000000000666 ) ;
#5791 = AXIS2_PLACEMENT_3D ( 'NONE', #13715, #2975, #5451 ) ;
#5792 = AXIS2_PLACEMENT_3D ( 'NONE', #9947, #12169, #10903 ) ;
#5793 = CARTESIAN_POINT ( 'NONE',  ( -2.961146025923796721, 227.1224618315849852, 6.835633734209157986 ) ) ;
#5794 = CARTESIAN_POINT ( 'NONE',  ( 5.770288754215171956, 2.404361317819856403, 25.37381964045071214 ) ) ;
#5795 = CARTESIAN_POINT ( 'NONE',  ( -2.500000000000000444, 185.9800000002184674, 8.035533905932737753 ) ) ;
#5796 = DIRECTION ( 'NONE',  ( -0.000000000000000000, 1.000000000000000000, -0.000000000000000000 ) ) ;
#5797 = CARTESIAN_POINT ( 'NONE',  ( 1.618192118698865700, 228.6399984490590214, 8.087742880769061671 ) ) ;
#5798 = FACE_BOUND ( 'NONE', #7414, .T. ) ;
#5799 = CARTESIAN_POINT ( 'NONE',  ( -1.461580736456472795, 1.461580736456472795, -0.2499999989075251672 ) ) ;
#5800 = CARTESIAN_POINT ( 'NONE',  ( 0.000000000000000000, 0.000000000000000000, 36.00000000000000711 ) ) ;
#5801 = VERTEX_POINT ( 'NONE', #10464 ) ;
#5802 = CARTESIAN_POINT ( 'NONE',  ( -0.8561741729129470624, 185.5999999989075206, 9.066987300000000971 ) ) ;
#5803 = CARTESIAN_POINT ( 'NONE',  ( -4.946672411965113980E-16, 184.5999999999999943, 9.500000000000001776 ) ) ;
#5804 = CIRCLE ( 'NONE', #3502, 12.50000000000000355 ) ;
#5805 = ADVANCED_FACE ( 'NONE', ( #12838 ), #15319, .T. ) ;
#5806 = ORIENTED_EDGE ( 'NONE', *, *, #9305, .T. ) ;
#5807 =( BOUNDED_SURFACE ( )  B_SPLINE_SURFACE ( 1, 2, ( 
 ( #1848, #5373, #14094, #8061, #10217, #5295, #5523, #4323, #15070, #2896, #10370, #15221, #14021, #3128, #12821, #1925, #12592, #6798, #735, #5602, #4085, #10448, #15302, #4405, #3203, #1616, #6492, #8956, #13788, #8142, #8299, #3515, #9654, #8221, #14410, #6953, #11944, #14321, #10834, #12902, #15616, #10600, #13056, #5755, #2080, #14245, #9409, #4477, #15380, #15696, #2236, #7107, #1126, #2155, #2316, #6878, #5991, #13223, #4718, #9568, #7029, #887, #11785, #2003, #3278, #3354, #5834, #15460, #11857, #13137, #969, #1049, #9330, #5679, #4800, #5912, #15539, #11711, #10759, #4561, #8385, #10679, #3430, #4636, #9490, #7188, #812, #12027, #14495, #3593, #10526, #14173, #12977, #14575, #6235, #9811, #11150, #3902, #5033, #4879, #5190, #6313, #11071, #252, #9737 ),
 ( #5112, #3671, #12184, #1436, #13373, #2483, #12261, #7419, #10043, #1282, #17, #8548, #171, #1202, #9965, #6075, #14816, #9888, #8776, #7493, #14740, #1361, #3827, #7265, #4960, #11227, #14893, #13533, #6393, #13607, #7342, #6156, #10995, #14660, #13301, #8466, #2397, #8700, #94, #2719, #3748, #8624, #2641, #12340, #12102, #13459, #2562, #7571, #12419, #10919, #1517, #329, #1828, #560, #6702, #3032, #5428, #12653, #11457, #2798, #483, #6778, #713, #9091, #1904, #15204, #8934, #4064, #11306, #5352, #8856, #5584, #13689, #10273, #1672, #9165, #10198, #12802, #7962, #3108, #15125, #11613, #12573, #2876, #3979, #7648, #11532, #632, #4303, #12496, #5505, #10431, #4222, #9014, #7723, #6473, #6547, #13767, #11381, #15048, #13920, #6625, #14000, #4141, #1595 ),
 ( #7885, #13843, #403, #5273, #2955, #10349, #10121, #7803, #1751, #14973, #12726, #5974, #2299, #14228, #5816, #870, #4385, #9471, #11694, #1110, #4458, #2060, #12960, #12878, #6936, #14302, #9553, #14153, #2217, #9239, #14074, #8122, #7169, #14391, #3495, #8203, #11839, #5736, #13206, #1985, #3335, #9313, #12007, #15282, #3256, #3184, #10659, #7088, #11767, #794, #7009, #949, #3411, #15519, #10580, #11924, #5660, #15440, #8282, #8042, #6858, #10507, #4618, #4540, #4701, #9390, #8366, #15362, #13039, #13116, #2136, #1029, #5893, #10740, #15600, #2621, #8683, #6291, #3575, #7477, #2699, #11053, #75, #9719, #13282, #13358, #4862, #14556, #3652, #2546, #13443, #5095, #12167, #9946, #2463, #8529, #9793, #12243, #1343, #1264, #8447, #11132, #7326, #12321, #14798 ) ),
 .UNSPECIFIED., .F., .F., .F. ) 
 B_SPLINE_SURFACE_WITH_KNOTS ( ( 2, 1, 2 ),
 ( 3, 2, 2, 2, 2, 2, 2, 2, 2, 2, 2, 2, 2, 2, 2, 2, 2, 2, 2, 2, 2, 2, 2, 2, 2, 2, 2, 2, 2, 2, 2, 2, 2, 2, 2, 2, 2, 2, 2, 2, 2, 2, 2, 2, 2, 2, 2, 2, 2, 2, 2, 2, 3 ),
 ( -0.01000000000000000021, 0.000000000000000000, 1.000000000000000000 ),
 ( -0.008928571428571429811, 0.000000000000000000, 0.01785714285714285615, 0.03571428571428571230, 0.05357142857142856845, 0.07142857142857142461, 0.08928571428571428770, 0.1071428571428571369, 0.1250000000000000000, 0.1428571428571428492, 0.1607142857142857262, 0.1785714285714285754, 0.1964285714285714246, 0.2142857142857142738, 0.2321428571428571508, 0.2500000000000000000, 0.2678571428571428492, 0.2857142857142856984, 0.3035714285714285476, 0.3214285714285714524, 0.3392857142857143016, 0.3571428571428571508, 0.3750000000000000000, 0.3928571428571428492, 0.4107142857142856984, 0.4285714285714285476, 0.4464285714285714524, 0.4642857142857143016, 0.4821428571428571508, 0.5000000000000000000, 0.5178571428571429047, 0.5357142857142856984, 0.5535714285714286031, 0.5714285714285713969, 0.5892857142857143016, 0.6071428571428570953, 0.6250000000000000000, 0.6428571428571429047, 0.6607142857142856984, 0.6785714285714286031, 0.6964285714285713969, 0.7142857142857143016, 0.7321428571428570953, 0.7500000000000000000, 0.7678571428571429047, 0.7857142857142856984, 0.8035714285714286031, 0.8214285714285713969, 0.8392857142857143016, 0.8571428571428570953, 0.8750000000000000000, 0.8928571428571429047, 0.9018750000000000933 ),
 .UNSPECIFIED. ) 
 GEOMETRIC_REPRESENTATION_ITEM ( )  RATIONAL_B_SPLINE_SURFACE ( (
 ( 1.000000000000000000, 1.000000000000000000, 1.000000000000000000, 0.9238795325112867385, 1.000000000000000000, 0.9238795325112867385, 1.000000000000000000, 0.9238795325112867385, 1.000000000000000000, 0.9238795325112867385, 1.000000000000000000, 0.9238795325112867385, 1.000000000000000000, 0.9238795325112867385, 1.000000000000000000, 0.9238795325112867385, 1.000000000000000000, 0.9238795325112867385, 1.000000000000000000, 0.9238795325112867385, 1.000000000000000000, 0.9238795325112867385, 1.000000000000000000, 0.9238795325112867385, 1.000000000000000000, 0.9238795325112867385, 1.000000000000000000, 0.9238795325112867385, 1.000000000000000000, 0.9238795325112867385, 1.000000000000000000, 0.9238795325112867385, 1.000000000000000000, 0.9238795325112867385, 1.000000000000000000, 0.9238795325112867385, 1.000000000000000000, 0.9238795325112867385, 1.000000000000000000, 0.9238795325112867385, 1.000000000000000000, 0.9238795325112867385, 1.000000000000000000, 0.9238795325112867385, 1.000000000000000000, 0.9238795325112867385, 1.000000000000000000, 0.9238795325112867385, 1.000000000000000000, 0.9238795325112867385, 1.000000000000000000, 0.9238795325112867385, 1.000000000000000000, 0.9238795325112867385, 1.000000000000000000, 0.9238795325112867385, 1.000000000000000000, 0.9238795325112867385, 1.000000000000000000, 0.9238795325112867385, 1.000000000000000000, 0.9238795325112867385, 1.000000000000000000, 0.9238795325112867385, 1.000000000000000000, 0.9238795325112867385, 1.000000000000000000, 0.9238795325112867385, 1.000000000000000000, 0.9238795325112867385, 1.000000000000000000, 0.9238795325112867385, 1.000000000000000000, 0.9238795325112867385, 1.000000000000000000, 0.9238795325112867385, 1.000000000000000000, 0.9238795325112867385, 1.000000000000000000, 0.9238795325112867385, 1.000000000000000000, 0.9238795325112867385, 1.000000000000000000, 0.9238795325112867385, 1.000000000000000000, 0.9238795325112867385, 1.000000000000000000, 0.9238795325112867385, 1.000000000000000000, 0.9238795325112867385, 1.000000000000000000, 0.9238795325112867385, 1.000000000000000000, 0.9238795325112867385, 1.000000000000000000, 0.9238795325112867385, 1.000000000000000000, 0.9238795325112867385, 1.000000000000000000, 0.9238795325112867385, 1.000000000000000000, 0.9238795325112867385, 1.000000000000000000, 1.000000000000000000, 1.000000000000000000),
 ( 1.000000000000000000, 1.000000000000000000, 1.000000000000000000, 0.9238795325112867385, 1.000000000000000000, 0.9238795325112867385, 1.000000000000000000, 0.9238795325112867385, 1.000000000000000000, 0.9238795325112867385, 1.000000000000000000, 0.9238795325112867385, 1.000000000000000000, 0.9238795325112867385, 1.000000000000000000, 0.9238795325112867385, 1.000000000000000000, 0.9238795325112867385, 1.000000000000000000, 0.9238795325112867385, 1.000000000000000000, 0.9238795325112867385, 1.000000000000000000, 0.9238795325112867385, 1.000000000000000000, 0.9238795325112867385, 1.000000000000000000, 0.9238795325112867385, 1.000000000000000000, 0.9238795325112867385, 1.000000000000000000, 0.9238795325112867385, 1.000000000000000000, 0.9238795325112867385, 1.000000000000000000, 0.9238795325112867385, 1.000000000000000000, 0.9238795325112867385, 1.000000000000000000, 0.9238795325112867385, 1.000000000000000000, 0.9238795325112867385, 1.000000000000000000, 0.9238795325112867385, 1.000000000000000000, 0.9238795325112867385, 1.000000000000000000, 0.9238795325112867385, 1.000000000000000000, 0.9238795325112867385, 1.000000000000000000, 0.9238795325112867385, 1.000000000000000000, 0.9238795325112867385, 1.000000000000000000, 0.9238795325112867385, 1.000000000000000000, 0.9238795325112867385, 1.000000000000000000, 0.9238795325112867385, 1.000000000000000000, 0.9238795325112867385, 1.000000000000000000, 0.9238795325112867385, 1.000000000000000000, 0.9238795325112867385, 1.000000000000000000, 0.9238795325112867385, 1.000000000000000000, 0.9238795325112867385, 1.000000000000000000, 0.9238795325112867385, 1.000000000000000000, 0.9238795325112867385, 1.000000000000000000, 0.9238795325112867385, 1.000000000000000000, 0.9238795325112867385, 1.000000000000000000, 0.9238795325112867385, 1.000000000000000000, 0.9238795325112867385, 1.000000000000000000, 0.9238795325112867385, 1.000000000000000000, 0.9238795325112867385, 1.000000000000000000, 0.9238795325112867385, 1.000000000000000000, 0.9238795325112867385, 1.000000000000000000, 0.9238795325112867385, 1.000000000000000000, 0.9238795325112867385, 1.000000000000000000, 0.9238795325112867385, 1.000000000000000000, 0.9238795325112867385, 1.000000000000000000, 0.9238795325112867385, 1.000000000000000000, 0.9238795325112867385, 1.000000000000000000, 1.000000000000000000, 1.000000000000000000),
 ( 1.000000000000000000, 1.000000000000000000, 1.000000000000000000, 0.9238795325112867385, 1.000000000000000000, 0.9238795325112867385, 1.000000000000000000, 0.9238795325112867385, 1.000000000000000000, 0.9238795325112867385, 1.000000000000000000, 0.9238795325112867385, 1.000000000000000000, 0.9238795325112867385, 1.000000000000000000, 0.9238795325112867385, 1.000000000000000000, 0.9238795325112867385, 1.000000000000000000, 0.9238795325112867385, 1.000000000000000000, 0.9238795325112867385, 1.000000000000000000, 0.9238795325112867385, 1.000000000000000000, 0.9238795325112867385, 1.000000000000000000, 0.9238795325112867385, 1.000000000000000000, 0.9238795325112867385, 1.000000000000000000, 0.9238795325112867385, 1.000000000000000000, 0.9238795325112867385, 1.000000000000000000, 0.9238795325112867385, 1.000000000000000000, 0.9238795325112867385, 1.000000000000000000, 0.9238795325112867385, 1.000000000000000000, 0.9238795325112867385, 1.000000000000000000, 0.9238795325112867385, 1.000000000000000000, 0.9238795325112867385, 1.000000000000000000, 0.9238795325112867385, 1.000000000000000000, 0.9238795325112867385, 1.000000000000000000, 0.9238795325112867385, 1.000000000000000000, 0.9238795325112867385, 1.000000000000000000, 0.9238795325112867385, 1.000000000000000000, 0.9238795325112867385, 1.000000000000000000, 0.9238795325112867385, 1.000000000000000000, 0.9238795325112867385, 1.000000000000000000, 0.9238795325112867385, 1.000000000000000000, 0.9238795325112867385, 1.000000000000000000, 0.9238795325112867385, 1.000000000000000000, 0.9238795325112867385, 1.000000000000000000, 0.9238795325112867385, 1.000000000000000000, 0.9238795325112867385, 1.000000000000000000, 0.9238795325112867385, 1.000000000000000000, 0.9238795325112867385, 1.000000000000000000, 0.9238795325112867385, 1.000000000000000000, 0.9238795325112867385, 1.000000000000000000, 0.9238795325112867385, 1.000000000000000000, 0.9238795325112867385, 1.000000000000000000, 0.9238795325112867385, 1.000000000000000000, 0.9238795325112867385, 1.000000000000000000, 0.9238795325112867385, 1.000000000000000000, 0.9238795325112867385, 1.000000000000000000, 0.9238795325112867385, 1.000000000000000000, 0.9238795325112867385, 1.000000000000000000, 0.9238795325112867385, 1.000000000000000000, 0.9238795325112867385, 1.000000000000000000, 1.000000000000000000, 1.000000000000000000) ) ) 
 REPRESENTATION_ITEM ( '' )  SURFACE ( )  );
#5808 = EDGE_CURVE ( 'NONE', #6636, #15622, #3216, .T. ) ;
#5809 = DIRECTION ( 'NONE',  ( -6.123233995736766036E-17, 1.000000000000000000, 0.000000000000000000 ) ) ;
#5810 = CARTESIAN_POINT ( 'NONE',  ( -2.668367453516725885, 5.373994336898083368, 31.00000000000000000 ) ) ;
#5811 = EDGE_CURVE ( 'NONE', #5746, #3666, #9981, .T. ) ;
#5812 = LINE ( 'NONE', #10577, #11114 ) ;
#5813 = CARTESIAN_POINT ( 'NONE',  ( 2.066987300000000527, 186.6499999989075320, 7.000000000000000000 ) ) ;
#5814 = CIRCLE ( 'NONE', #15212, 2.750000000000002665 ) ;
#5815 = CARTESIAN_POINT ( 'NONE',  ( 2.668367453516584664, -5.373994336898154422, 18.13061695532137918 ) ) ;
#5816 = CARTESIAN_POINT ( 'NONE',  ( 4.592425496802573972E-16, -2.500000000000000000, 1.200000002184949732 ) ) ;
#5817 = AXIS2_PLACEMENT_3D ( 'NONE', #15552, #30, #6386 ) ;
#5818 = CARTESIAN_POINT ( 'NONE',  ( -6.081509788407743144, -1.446521464462711570, 4.126180359549291410 ) ) ;
#5819 = CARTESIAN_POINT ( 'NONE',  ( 5.999999999999999112, 229.2449477060184222, 9.834870838912449287 ) ) ;
#5820 = CARTESIAN_POINT ( 'NONE',  ( 2.500000000000000000, 3.061616997868383141E-16, 0.5000000000000000000 ) ) ;
#5821 = CYLINDRICAL_SURFACE ( 'NONE', #14125, 1.999999999999999556 ) ;
#5822 = CARTESIAN_POINT ( 'NONE',  ( 5.747343991580187605, 1.727858744772266419, 12.49992002356259668 ) ) ;
#5823 = ORIENTED_EDGE ( 'NONE', *, *, #3135, .T. ) ;
#5824 = EDGE_LOOP ( 'NONE', ( #6885, #5141, #9172, #6692 ) ) ;
#5825 = AXIS2_PLACEMENT_3D ( 'NONE', #7839, #6966, #3142 ) ;
#5826 = VERTEX_POINT ( 'NONE', #9585 ) ;
#5827 = CARTESIAN_POINT ( 'NONE',  ( 3.726944967918921492E-17, 185.4499999989075150, 4.933012699999999029 ) ) ;
#5828 = CARTESIAN_POINT ( 'NONE',  ( -2.500000000000000444, 184.0000000000000000, 7.000000000000000000 ) ) ;
#5829 = ORIENTED_EDGE ( 'NONE', *, *, #494, .F. ) ;
#5830 = CARTESIAN_POINT ( 'NONE',  ( 1.767766952966369320, -1.767766952966368654, -1.899999997815050579 ) ) ;
#5831 = CARTESIAN_POINT ( 'NONE',  ( -0.2619456584319997949, 5.995505046955622142, 23.52607193928647433 ) ) ;
#5832 = CARTESIAN_POINT ( 'NONE',  ( 4.435347140100866170, 4.403429997944680707, 24.63237410716306286 ) ) ;
#5833 = CARTESIAN_POINT ( 'NONE',  ( 0.8561741729129452860, 187.7999999989075093, 4.933012699999999029 ) ) ;
#5834 = CARTESIAN_POINT ( 'NONE',  ( -2.500000000000000000, 0.000000000000000000, -0.6930000000218496936 ) ) ;
#5835 = CARTESIAN_POINT ( 'NONE',  ( 5.317509234263995133, 2.779225709350928053, 17.99999999999998934 ) ) ;
#5836 = CONTEXT_DEPENDENT_SHAPE_REPRESENTATION ( #2097, #9325 ) ;
#5837 = CARTESIAN_POINT ( 'NONE',  ( 0.8561741729129451750, 2.066987299999999639, 0.2000000010924747329 ) ) ;
#5838 = DIRECTION ( 'NONE',  ( 0.000000000000000000, 0.000000000000000000, 1.000000000000000000 ) ) ;
#5839 = CARTESIAN_POINT ( 'NONE',  ( 2.840695628781289894, 227.6003006331432346, 8.242276837941533429 ) ) ;
#5840 = CARTESIAN_POINT ( 'NONE',  ( -1.827163138824825950, 228.0559401102076151, 9.582586618047248095 ) ) ;
#5841 = ORIENTED_EDGE ( 'NONE', *, *, #6538, .T. ) ;
#5842 = FACE_OUTER_BOUND ( 'NONE', #3582, .T. ) ;
#5843 = ORIENTED_EDGE ( 'NONE', *, *, #8342, .F. ) ;
#5844 = EDGE_LOOP ( 'NONE', ( #11525, #10112 ) ) ;
#5845 = CARTESIAN_POINT ( 'NONE',  ( -5.858813228503639614, -2.179803269293304258, 30.02622717124732077 ) ) ;
#5846 = CARTESIAN_POINT ( 'NONE',  ( -4.344502777243634206, -4.493369211529165241, 23.99610786875030755 ) ) ;
#5847 = CARTESIAN_POINT ( 'NONE',  ( -3.420311045507915981, -4.931422832349241503, 25.50007961174475923 ) ) ;
#5848 = EDGE_CURVE ( 'NONE', #5672, #13817, #12746, .T. ) ;
#5849 = ORIENTED_EDGE ( 'NONE', *, *, #771, .F. ) ;
#5850 = CARTESIAN_POINT ( 'NONE',  ( -6.172639027853117355, -0.9816353142771756524, 31.26225281721713145 ) ) ;
#5851 = UNCERTAINTY_MEASURE_WITH_UNIT (LENGTH_MEASURE( 1.000000000000000082E-05 ), #6210, 'distance_accuracy_value', 'NONE');
#5852 = CARTESIAN_POINT ( 'NONE',  ( -0.7995524673975737961, -6.199337389817267230, 5.614536794524584984 ) ) ;
#5853 = CARTESIAN_POINT ( 'NONE',  ( -0.8730628416135229886, -6.188929913094992408, 23.99504929893116056 ) ) ;
#5854 = CARTESIAN_POINT ( 'NONE',  ( -2.817313151351230172, -5.579000502529412486, 17.99999999999998934 ) ) ;
#5855 = CARTESIAN_POINT ( 'NONE',  ( 0.6139908388542412165, -5.969238533166598693, 17.19977627912011542 ) ) ;
#5856 = CARTESIAN_POINT ( 'NONE',  ( 5.131373506000599605, 7.062729720844090231, 5.000000000000004441 ) ) ;
#5857 = CARTESIAN_POINT ( 'NONE',  ( 0.002394265188360167329, 0.4000000000000062395, -2.473000379418545780 ) ) ;
#5858 = CARTESIAN_POINT ( 'NONE',  ( 2.500000000000000000, 189.4999999978150527, 7.000000000000000000 ) ) ;
#5859 = CARTESIAN_POINT ( 'NONE',  ( 1.498625850689462968, 228.1261123260860018, 9.788931089129667029 ) ) ;
#5860 = CARTESIAN_POINT ( 'NONE',  ( -5.984595133899131447, -1.806709459528820227, 18.99995078984292007 ) ) ;
#5861 = DIRECTION ( 'NONE',  ( -0.000000000000000000, 1.000000000000000000, -0.000000000000000000 ) ) ;
#5862 = EDGE_LOOP ( 'NONE', ( #3795, #9580 ) ) ;
#5863 = CARTESIAN_POINT ( 'NONE',  ( -5.375605342016499755, 2.665598297262299354, 12.00312048902375217 ) ) ;
#5864 = CARTESIAN_POINT ( 'NONE',  ( 6.780834053290958173E-14, -6.000000000000000888, 10.49999999999998224 ) ) ;
#5866 = ORIENTED_EDGE ( 'NONE', *, *, #6453, .F. ) ;
#5865 = CARTESIAN_POINT ( 'NONE',  ( -0.2624013748571158433, -5.995472630654528956, 23.52628559691083154 ) ) ;
#5867 = DIRECTION ( 'NONE',  ( 0.000000000000000000, 0.000000000000000000, -1.000000000000000000 ) ) ;
#5868 = CARTESIAN_POINT ( 'NONE',  ( 0.2023276174660176285, 0.4000000000000061839, 2.561683098399134106 ) ) ;
#5869 = ORIENTED_EDGE ( 'NONE', *, *, #7266, .F. ) ;
#5870 = CARTESIAN_POINT ( 'NONE',  ( 0.000000000000000000, 22.00000000000000000, 0.000000000000000000 ) ) ;
#5871 = B_SPLINE_CURVE_WITH_KNOTS ( 'NONE', 3,
 ( #11435, #536, #5404, #10252, #15104, #6010, #7205, #9069, #11962, #6756, #4578, #1880, #13979, #10619, #8405, #7044, #15180, #2256 ),
 .UNSPECIFIED., .F., .F.,
 ( 4, 2, 2, 2, 2, 2, 2, 2, 4 ),
 ( 0.003131918686235972589, 0.003523310662250263292, 0.003914702638264553995, 0.004306094614278844698, 0.004697486590293136269, 0.005088878566307426105, 0.005480270542321717675, 0.005871662518336008378, 0.006263054494350299081 ),
 .UNSPECIFIED. ) ;
#5872 = CARTESIAN_POINT ( 'NONE',  ( -1.461580736456472351, -1.461580736456473018, 1.550000001092474822 ) ) ;
#5873 = CARTESIAN_POINT ( 'NONE',  ( -2.735089344010680268, 227.6862984522302611, 8.495314001923839342 ) ) ;
#5874 = FACE_OUTER_BOUND ( 'NONE', #11847, .T. ) ;
#5875 = CARTESIAN_POINT ( 'NONE',  ( 2.500000000000000444, 184.7300000002184959, 7.000000000000000000 ) ) ;
#5876 = FACE_OUTER_BOUND ( 'NONE', #8990, .T. ) ;
#5877 = APPLICATION_CONTEXT ( 'automotive_design' ) ;
#5878 = CARTESIAN_POINT ( 'NONE',  ( 0.9680444063220374762, 227.6910878243089087, 5.347234874174658259 ) ) ;
#5879 = FACE_OUTER_BOUND ( 'NONE', #7219, .T. ) ;
#5880 = CARTESIAN_POINT ( 'NONE',  ( 2.066987300000000083, -0.8561741729129450640, 1.000000001092474777 ) ) ;
#5881 = CARTESIAN_POINT ( 'NONE',  ( -5.000000000000000000, 0.000000000000000000, 5.000000000000004441 ) ) ;
#5882 = ORIENTED_EDGE ( 'NONE', *, *, #5519, .F. ) ;
#5883 = CARTESIAN_POINT ( 'NONE',  ( 1.461580736456473240, 188.3499999989074922, 5.538419263543526760 ) ) ;
#5884 = CARTESIAN_POINT ( 'NONE',  ( -2.066987300000001415, 185.4999999989075548, 7.856174172912944620 ) ) ;
#5885 = CARTESIAN_POINT ( 'NONE',  ( 5.329945432499665792, 2.755769831645062506, 24.23770962164067200 ) ) ;
#5886 = ORIENTED_EDGE ( 'NONE', *, *, #5618, .T. ) ;
#5887 = CARTESIAN_POINT ( 'NONE',  ( -3.061616997868391523E-16, 182.0000000000000000, -7.000000000000000000 ) ) ;
#5888 = CARTESIAN_POINT ( 'NONE',  ( 0.2622538972266198476, -6.245673238944467798, 25.47385994369200191 ) ) ;
#5889 = CARTESIAN_POINT ( 'NONE',  ( -2.500000000000000444, 1.035533905932737753, 0.1500000021849498544 ) ) ;
#5890 = LINE ( 'NONE', #9236, #5784 ) ;
#5891 = CARTESIAN_POINT ( 'NONE',  ( -0.8561741729129457301, 186.8999999989075320, 4.933012699999999029 ) ) ;
#5892 = CARTESIAN_POINT ( 'NONE',  ( 4.141923667210617666, -4.342011609040492104, 18.61561732698604743 ) ) ;
#5893 = CARTESIAN_POINT ( 'NONE',  ( 1.767766952966368654, 1.767766952966369098, -1.699999997815050179 ) ) ;
#5894 = DIRECTION ( 'NONE',  ( 0.000000000000000000, 0.000000000000000000, 1.000000000000000000 ) ) ;
#5895 = CARTESIAN_POINT ( 'NONE',  ( -1.500000000000000000, 9.750000000000003553, 2.000000000000001776 ) ) ;
#5896 = CARTESIAN_POINT ( 'NONE',  ( -5.935543223013851843, 0.8771126767607326791, 11.36760611998364823 ) ) ;
#5897 = CARTESIAN_POINT ( 'NONE',  ( 1.035533905932738419, 185.3499999978151038, 9.500000000000000000 ) ) ;
#5898 = CARTESIAN_POINT ( 'NONE',  ( -0.2638277032947476952, -5.995407492418047823, 18.97332055281517427 ) ) ;
#5899 = EDGE_CURVE ( 'NONE', #7142, #7332, #9410, .T. ) ;
#5900 = VERTEX_POINT ( 'NONE', #14511 ) ;
#5901 = ORIENTED_EDGE ( 'NONE', *, *, #9837, .T. ) ;
#5902 = EDGE_LOOP ( 'NONE', ( #3993, #4570 ) ) ;
#5903 = AXIS2_PLACEMENT_3D ( 'NONE', #1378, #188, #14431 ) ;
#5904 = CARTESIAN_POINT ( 'NONE',  ( 0.8561741729129456191, 184.5999999989075206, 4.933012699999999029 ) ) ;
#5905 = CARTESIAN_POINT ( 'NONE',  ( 1.224717432196171130, 227.7398333025587362, 5.488014595619924663 ) ) ;
#5906 = ORIENTED_EDGE ( 'NONE', *, *, #2821, .T. ) ;
#5907 = PRODUCT_DEFINITION_SHAPE ( 'NONE', 'NONE',  #15742 ) ;
#5908 = CARTESIAN_POINT ( 'NONE',  ( -1.035533905932738197, -2.500000000000000000, -2.049999997815050268 ) ) ;
#5909 = CARTESIAN_POINT ( 'NONE',  ( 6.155973317223301322, 1.081218830693648103, 18.50308643866044633 ) ) ;
#5910 = CARTESIAN_POINT ( 'NONE',  ( -4.322356511625880415, 7.650514973136431252, 17.99999999999998934 ) ) ;
#5911 = CARTESIAN_POINT ( 'NONE',  ( -1.592421940838084637E-16, 188.6499999989075320, 4.933012699999999029 ) ) ;
#5912 = CARTESIAN_POINT ( 'NONE',  ( 2.500000000000000444, -1.035533905932737309, -1.143000000021849427 ) ) ;
#5913 = CARTESIAN_POINT ( 'NONE',  ( 5.726049995854467944, -2.506679546901878552, 4.200455375311575423 ) ) ;
#5914 = EDGE_CURVE ( 'NONE', #3929, #11668, #7124, .T. ) ;
#5915 = CARTESIAN_POINT ( 'NONE',  ( 0.8561741729129463963, -2.066987299999999195, -0.8999999989075251339 ) ) ;
#5916 = VECTOR ( 'NONE', #670, 1000.000000000000000 ) ;
#5917 = CARTESIAN_POINT ( 'NONE',  ( 3.779681992289859682, -4.979315417303849856, 30.00004921015706216 ) ) ;
#5918 = CARTESIAN_POINT ( 'NONE',  ( 1.059913075168976260, 226.3867898013274669, 4.668296007112484602 ) ) ;
#5919 = CARTESIAN_POINT ( 'NONE',  ( 0.000000000000000000, 0.000000000000000000, 0.000000000000000000 ) ) ;
#5920 = EDGE_LOOP ( 'NONE', ( #14750, #1856, #9838, #5771 ) ) ;
#5921 = ORIENTED_EDGE ( 'NONE', *, *, #5922, .T. ) ;
#5922 = EDGE_CURVE ( 'NONE', #15454, #12751, #7136, .T. ) ;
#5923 = CARTESIAN_POINT ( 'NONE',  ( -2.500000000000000888, 188.2999999978150356, 7.000000000000000000 ) ) ;
#5924 = ORIENTED_EDGE ( 'NONE', *, *, #7856, .F. ) ;
#5925 = VERTEX_POINT ( 'NONE', #6008 ) ;
#5926 = CARTESIAN_POINT ( 'NONE',  ( -5.615811513734994875, -2.743665920700480765, 30.49691356133953590 ) ) ;
#5927 = CARTESIAN_POINT ( 'NONE',  ( 2.848235266350942929, -5.281699484015692114, 17.38602261056917797 ) ) ;
#5928 = CARTESIAN_POINT ( 'NONE',  ( 0.9999505860953422642, -6.169489349035806924, 5.131059031658107727 ) ) ;
#5929 = CARTESIAN_POINT ( 'NONE',  ( 3.311576095066596892, -5.004818610361295939, 12.47377823943291730 ) ) ;
#5930 = CARTESIAN_POINT ( 'NONE',  ( -1.000082492230715436, -6.169467968613708386, 5.131525381053921642 ) ) ;
#5931 = DIRECTION ( 'NONE',  ( 0.5877852522924802425, -0.8090169943749422332, 0.000000000000000000 ) ) ;
#5932 = CARTESIAN_POINT ( 'NONE',  ( -2.931212650151701293, -5.520239928492797432, 18.50425949503010514 ) ) ;
#5933 = CARTESIAN_POINT ( 'NONE',  ( -6.105861027178912437, -1.337741388557158073, 23.70045537531158075 ) ) ;
#5934 = DIRECTION ( 'NONE',  ( -1.000000000000000000, 3.326610055774637112E-18, 1.062480551894331163E-17 ) ) ;
#5935 = DIRECTION ( 'NONE',  ( 1.000000000000000000, 0.000000000000000000, 0.000000000000000000 ) ) ;
#5936 = CARTESIAN_POINT ( 'NONE',  ( 2.500000000000000444, 187.9499999978150697, 5.964466094067262247 ) ) ;
#5937 = CARTESIAN_POINT ( 'NONE',  ( 2.349311747835623354, 227.8901172732836642, 9.094898149752092209 ) ) ;
#5938 = CARTESIAN_POINT ( 'NONE',  ( 2.848235266350975792, 5.281699484015673463, 31.61397738943082203 ) ) ;
#5939 = EDGE_CURVE ( 'NONE', #12984, #15268, #15672, .T. ) ;
#5940 = EDGE_CURVE ( 'NONE', #9955, #7970, #11297, .T. ) ;
#5941 = CARTESIAN_POINT ( 'NONE',  ( -0.3590199077019145535, 189.4412677667518210, 3.993594655970155838 ) ) ;
#5942 = VERTEX_POINT ( 'NONE', #7741 ) ;
#5943 = CARTESIAN_POINT ( 'NONE',  ( 9.750000000000003553, 22.00000000000000000, 1.020968533498575335E-13 ) ) ;
#5944 = CARTESIAN_POINT ( 'NONE',  ( 0.8737888311110715289, -5.936248257219499003, 12.00344185141215192 ) ) ;
#5946 = ORIENTED_EDGE ( 'NONE', *, *, #4555, .F. ) ;
#5945 = CARTESIAN_POINT ( 'NONE',  ( -1.035533905932739751, 187.7500000000000284, 9.500000000000000000 ) ) ;
#5947 = CARTESIAN_POINT ( 'NONE',  ( 2.930600586413029784, -5.520563544161715797, 31.50308643866046054 ) ) ;
#5948 = CARTESIAN_POINT ( 'NONE',  ( 1.058049511578855073, 226.3870755470184122, 4.669134239153247101 ) ) ;
#5949 = CARTESIAN_POINT ( 'NONE',  ( -4.435347140101025154, -4.403429997944519947, 31.13060690723500201 ) ) ;
#5950 = VECTOR ( 'NONE', #621, 1000.000000000000114 ) ;
#5951 = CARTESIAN_POINT ( 'NONE',  ( -2.066987299999999195, -0.8561741729129466183, -0.8999999989075251339 ) ) ;
#5952 = CARTESIAN_POINT ( 'NONE',  ( -1.233820397871397523, 226.4104340690482218, 4.737993341516149925 ) ) ;
#5953 = SURFACE_STYLE_USAGE ( .BOTH. , #15342 ) ;
#5954 = CARTESIAN_POINT ( 'NONE',  ( -6.176542424588111757, 0.9554180641286129649, 11.63234125634166105 ) ) ;
#5955 = CARTESIAN_POINT ( 'NONE',  ( -1.035533905932737975, 188.1800000002185129, 4.500000000000000888 ) ) ;
#5956 = CARTESIAN_POINT ( 'NONE',  ( -3.255128505894301583, 5.336774832660725387, 5.873800552473966263 ) ) ;
#5957 = CARTESIAN_POINT ( 'NONE',  ( -0.6092285535620440839, 227.6401390286306992, 5.200091846327095979 ) ) ;
#5958 = CARTESIAN_POINT ( 'NONE',  ( -2.668367453516726329, 5.373994336898084256, 30.86763921416088863 ) ) ;
#5959 = CARTESIAN_POINT ( 'NONE',  ( 2.066987300000000083, -0.8561741729129450640, 0.2000000010924747329 ) ) ;
#5960 = CARTESIAN_POINT ( 'NONE',  ( 6.105747081304190083, 1.338335777572186469, 17.19973484982324763 ) ) ;
#5961 = VERTEX_POINT ( 'NONE', #7510 ) ;
#5962 = CARTESIAN_POINT ( 'NONE',  ( 1.461580736456472573, 188.1499999989075036, 8.461580736456474128 ) ) ;
#5963 = EDGE_CURVE ( 'NONE', #13449, #3041, #5368, .T. ) ;
#5964 = CARTESIAN_POINT ( 'NONE',  ( -4.302927372051845722E-16, 184.8499999989074922, 9.066987300000000971 ) ) ;
#5965 = CARTESIAN_POINT ( 'NONE',  ( 5.931828553037990837, 0.9033193133618145909, 24.23805675996852926 ) ) ;
#5966 = ORIENTED_EDGE ( 'NONE', *, *, #5329, .F. ) ;
#5967 = FILL_AREA_STYLE_COLOUR ( '', #7618 ) ;
#5968 = CIRCLE ( 'NONE', #11538, 2.000000000000000000 ) ;
#5969 = CARTESIAN_POINT ( 'NONE',  ( 0.8736772044962008987, -6.188841968496030965, 23.99611573292810718 ) ) ;
#5970 = LINE ( 'NONE', #5090, #13557 ) ;
#5971 = CARTESIAN_POINT ( 'NONE',  ( 5.999999999999999112, 195.9172377311516016, 6.220370292208427188 ) ) ;
#5972 = CARTESIAN_POINT ( 'NONE',  ( -2.066987300000001415, 187.8999999989075036, 7.856174172912944620 ) ) ;
#5973 = CARTESIAN_POINT ( 'NONE',  ( 2.692143549875461783, -5.362363179736447272, 30.73805675996853637 ) ) ;
#5974 = CARTESIAN_POINT ( 'NONE',  ( 2.500000000000000444, -1.035533905932737309, 1.350000002184949643 ) ) ;
#5975 = CARTESIAN_POINT ( 'NONE',  ( -0.9739805876847694721, -5.920636045238170553, 31.26171386814423414 ) ) ;
#5976 = DIRECTION ( 'NONE',  ( 0.000000000000000000, 0.000000000000000000, -1.000000000000000000 ) ) ;
#5977 = DIRECTION ( 'NONE',  ( -0.000000000000000000, -1.000000000000000000, -0.000000000000000000 ) ) ;
#5978 = LINE ( 'NONE', #13362, #1418 ) ;
#5979 = CARTESIAN_POINT ( 'NONE',  ( 2.692335458626711642, 5.362264153667302580, 24.23760108194402108 ) ) ;
#5980 = AXIS2_PLACEMENT_3D ( 'NONE', #4614, #9549, #13111 ) ;
#5981 = EDGE_CURVE ( 'NONE', #6465, #1423, #4856, .T. ) ;
#5982 = VERTEX_POINT ( 'NONE', #11166 ) ;
#5983 = ORIENTED_EDGE ( 'NONE', *, *, #42, .F. ) ;
#5984 = VERTEX_POINT ( 'NONE', #11086 ) ;
#5985 = FACE_OUTER_BOUND ( 'NONE', #12647, .T. ) ;
#5986 = ORIENTED_EDGE ( 'NONE', *, *, #2427, .T. ) ;
#5987 = CARTESIAN_POINT ( 'NONE',  ( 4.592425496802573972E-16, -2.500000000000000000, -2.799999997815050268 ) ) ;
#5988 = DIRECTION ( 'NONE',  ( 0.000000000000000000, -1.000000000000000000, 0.000000000000000000 ) ) ;
#5989 = CARTESIAN_POINT ( 'NONE',  ( -9.750000000000003553, 22.00000000000000000, -1.500000000000033751 ) ) ;
#5990 = CARTESIAN_POINT ( 'NONE',  ( -6.098637220230962441E-17, 187.0499999989075093, 4.933012699999999029 ) ) ;
#5991 = CARTESIAN_POINT ( 'NONE',  ( 1.767766952966368654, 1.767766952966369098, -0.1930000000218495826 ) ) ;
#5992 =( REPRESENTATION_RELATIONSHIP ('NONE','NONE', #11191, #4596 ) REPRESENTATION_RELATIONSHIP_WITH_TRANSFORMATION ( #1284 )SHAPE_REPRESENTATION_RELATIONSHIP( ) );
#5993 = CARTESIAN_POINT ( 'NONE',  ( -2.500000000000000444, 185.2000000000000171, 7.000000000000000000 ) ) ;
#5994 = CARTESIAN_POINT ( 'NONE',  ( 2.066987299999999639, 2.531329380823229670E-16, 1.850000001092474866 ) ) ;
#5995 = CARTESIAN_POINT ( 'NONE',  ( 4.069684453406374303, -4.744965295353490653, 4.126199447526043507 ) ) ;
#5996 = CARTESIAN_POINT ( 'NONE',  ( -2.961755302830887615, 227.1327330595862861, 6.865988109554851171 ) ) ;
#5997 = CARTESIAN_POINT ( 'NONE',  ( 6.768587589771821120E-14, -6.250000000000000888, 12.49999999999998401 ) ) ;
#5998 = ORIENTED_EDGE ( 'NONE', *, *, #1371, .F. ) ;
#5999 = VERTEX_POINT ( 'NONE', #6409 ) ;
#6000 = CARTESIAN_POINT ( 'NONE',  ( 2.500000000000000444, 186.2999999978150356, 7.000000000000000000 ) ) ;
#6001 = VERTEX_POINT ( 'NONE', #6486 ) ;
#6002 = VERTEX_POINT ( 'NONE', #8794 ) ;
#6003 = DIRECTION ( 'NONE',  ( 1.000000000000000000, 0.000000000000000000, 0.000000000000000000 ) ) ;
#6004 = EDGE_CURVE ( 'NONE', #11257, #15393, #1233, .T. ) ;
#6005 = FACE_BOUND ( 'NONE', #7392, .T. ) ;
#6006 = CARTESIAN_POINT ( 'NONE',  ( -2.500000000000000444, 185.0999999978150754, 7.000000000000000000 ) ) ;
#6007 = ADVANCED_FACE ( 'NONE', ( #12895 ), #8991, .T. ) ;
#6008 = CARTESIAN_POINT ( 'NONE',  ( 6.176542424588105540, 0.9554180641286316167, 5.000000000000004441 ) ) ;
#6009 = UNCERTAINTY_MEASURE_WITH_UNIT (LENGTH_MEASURE( 1.000000000000000082E-05 ), #6118, 'distance_accuracy_value', 'NONE');
#6010 = CARTESIAN_POINT ( 'NONE',  ( 5.867109477881265356, -1.259218163100813026, 17.20111757752057713 ) ) ;
#6011 = CARTESIAN_POINT ( 'NONE',  ( -4.006441409774713414, -4.467329318258233428, 12.29888242247937669 ) ) ;
#6012 = CARTESIAN_POINT ( 'NONE',  ( 0.000000000000000000, -0.001000000000000132727, -13.50000000000000000 ) ) ;
#6013 = AXIS2_PLACEMENT_3D ( 'NONE', #12451, #8969, #1551 ) ;
#6014 = CARTESIAN_POINT ( 'NONE',  ( -2.500000000000000444, 1.035533905932737753, -2.350000000000000533 ) ) ;
#6015 = CARTESIAN_POINT ( 'NONE',  ( 1.035533905932737753, 188.1499999999999773, 4.500000000000001776 ) ) ;
#6016 = CARTESIAN_POINT ( 'NONE',  ( 0.02480202873542981801, 0.000000000000000000, 0.000000000000000000 ) ) ;
#6017 = PRODUCT ( 'pneumatic air inlet fitting', 'pneumatic air inlet fitting', '', ( #1850 ) ) ;
#6018 = CARTESIAN_POINT ( 'NONE',  ( 2.500000000000000444, 187.8999999978150584, 7.000000000000000000 ) ) ;
#6019 = CARTESIAN_POINT ( 'NONE',  ( 2.840695628781289894, 227.6003006331432346, 8.242276837941533429 ) ) ;
#6020 = CARTESIAN_POINT ( 'NONE',  ( 5.558508435838291462, -2.857531096718732844, 17.86765874365829276 ) ) ;
#6021 = EDGE_CURVE ( 'NONE', #1290, #10824, #9011, .T. ) ;
#6022 = CARTESIAN_POINT ( 'NONE',  ( -0.1252076328335900435, 190.0879680885402934, 4.197210855963412257 ) ) ;
#6023 = ORIENTED_EDGE ( 'NONE', *, *, #4237, .T. ) ;
#6024 = CARTESIAN_POINT ( 'NONE',  ( 3.061616997868383141E-16, 0.000000000000000000, 2.500000000000000000 ) ) ;
#6025 = CARTESIAN_POINT ( 'NONE',  ( 0.9740807849836848886, -5.920620690450679291, 11.23850119700669126 ) ) ;
#6027 = EDGE_LOOP ( 'NONE', ( #15025, #495 ) ) ;
#6026 = CARTESIAN_POINT ( 'NONE',  ( 1.767766952966368432, 187.8999999999999773, 8.767766952966368876 ) ) ;
#6028 = CARTESIAN_POINT ( 'NONE',  ( 4.290130679986615903, -4.545972905167685596, 31.61560192892919829 ) ) ;
#6029 = CARTESIAN_POINT ( 'NONE',  ( 2.449293598294708880E-16, 0.000000000000000000, -15.50000000000000000 ) ) ;
#6030 = ORIENTED_EDGE ( 'NONE', *, *, #9396, .F. ) ;
#6031 = CARTESIAN_POINT ( 'NONE',  ( 4.435347140100866170, 4.403429997944678931, 24.36765874365828921 ) ) ;
#6032 = CARTESIAN_POINT ( 'NONE',  ( 1.461580736456472573, 1.461580736456472795, 0.3500000010924749216 ) ) ;
#6033 = CARTESIAN_POINT ( 'NONE',  ( -0.1892923005757740362, 226.3252034129036474, 4.486734984831129758 ) ) ;
#6034 =( LENGTH_UNIT ( ) NAMED_UNIT ( * ) SI_UNIT ( .MILLI., .METRE. ) );
#6035 = DIRECTION ( 'NONE',  ( 0.9510565162951499785, 0.3090169943749582204, 0.000000000000000000 ) ) ;
#6036 = CARTESIAN_POINT ( 'NONE',  ( 2.500000000000000444, 188.7800000002184788, 5.964466094067262247 ) ) ;
#6037 = CARTESIAN_POINT ( 'NONE',  ( -1.592074373690287370, 228.6606520933046340, 8.147391783356672690 ) ) ;
#6038 = CIRCLE ( 'NONE', #13391, 3.118365096457674124 ) ;
#6039 = CARTESIAN_POINT ( 'NONE',  ( 1.984332343511774788, 228.2073501340537973, 6.838229870390527765 ) ) ;
#6040 = CARTESIAN_POINT ( 'NONE',  ( 2.066987300000000083, -0.8561741729129450640, -0.5999999989075253115 ) ) ;
#6041 = CARTESIAN_POINT ( 'NONE',  ( 0.000000000000000000, 0.000000000000000000, -5.500000000000000000 ) ) ;
#6042 = VERTEX_POINT ( 'NONE', #4676 ) ;
#6043 = CARTESIAN_POINT ( 'NONE',  ( -1.461580736456473906, 187.9499999989075150, 8.461580736456474128 ) ) ;
#6044 = CARTESIAN_POINT ( 'NONE',  ( -0.8561741729129457301, 186.0999999989074922, 4.933012699999999029 ) ) ;
#6045 = CARTESIAN_POINT ( 'NONE',  ( -5.940390500375658078, 6.474944468551550258, 5.000000000000004441 ) ) ;
#6046 = CARTESIAN_POINT ( 'NONE',  ( -1.767766952966369098, 1.767766952966369098, 1.599999999999999867 ) ) ;
#6047 = ORIENTED_EDGE ( 'NONE', *, *, #13102, .F. ) ;
#6048 = CARTESIAN_POINT ( 'NONE',  ( -3.011139120916623391, -5.190534000030277539, 23.70068193741825624 ) ) ;
#6049 = VECTOR ( 'NONE', #8913, 1000.000000000000114 ) ;
#6050 = CARTESIAN_POINT ( 'NONE',  ( 5.317509234263970264, -2.779225709350972906, 5.000000000000004441 ) ) ;
#6051 = EDGE_CURVE ( 'NONE', #13870, #9028, #1837, .T. ) ;
#6052 = B_SPLINE_CURVE_WITH_KNOTS ( 'NONE', 3,
 ( #5096, #6140, #7327, #12244, #6219, #14479, #10977, #76, #11054, #153, #5975, #5017, #2382, #1111, #9871, #3811, #8684, #3576 ),
 .UNSPECIFIED., .F., .F.,
 ( 4, 2, 2, 2, 2, 2, 2, 2, 4 ),
 ( 0.003131923598876997471, 0.003523316383094313945, 0.003914709167311630419, 0.004306101951528946460, 0.004697494735746262501, 0.005088887519963579409, 0.005480280304180895450, 0.005871673088398211490, 0.006263065872615528398 ),
 .UNSPECIFIED. ) ;
#6053 = DIRECTION ( 'NONE',  ( -1.000000000000000000, 0.000000000000000000, 0.000000000000000000 ) ) ;
#6054 = CARTESIAN_POINT ( 'NONE',  ( 0.000000000000000000, 6.250000000000000888, 12.49999999999998401 ) ) ;
#6055 = CARTESIAN_POINT ( 'NONE',  ( -0.7995524673974949703, -6.199337389817277000, 12.11453679452457521 ) ) ;
#6056 = CARTESIAN_POINT ( 'NONE',  ( 3.922288969639678768, 4.542045818322613115, 18.87378430870261781 ) ) ;
#6057 = CARTESIAN_POINT ( 'NONE',  ( 1.304322108239046818, 189.7221164505237425, 10.09240358076341693 ) ) ;
#6058 = CARTESIAN_POINT ( 'NONE',  ( -5.317509234263906315, 2.779225709351095475, 17.99999999999998934 ) ) ;
#6059 = CARTESIAN_POINT ( 'NONE',  ( 5.486982057989192363, -2.429327048029870539, 31.79931806258174376 ) ) ;
#6061 = CARTESIAN_POINT ( 'NONE',  ( -4.290821322214410038, 4.545321419741521929, 30.38558052754516225 ) ) ;
#6060 = AXIS2_PLACEMENT_3D ( 'NONE', #14965, #9956, #319 ) ;
#6062 = CARTESIAN_POINT ( 'NONE',  ( -6.105925084677696013, 1.337450587213117048, 10.70066851092422233 ) ) ;
#6063 = DIRECTION ( 'NONE',  ( 0.000000000000000000, 0.000000000000000000, 1.000000000000000000 ) ) ;
#6064 = AXIS2_PLACEMENT_3D ( 'NONE', #10256, #5409, #6606 ) ;
#6065 = ORIENTED_EDGE ( 'NONE', *, *, #13730, .F. ) ;
#6066 = VERTEX_POINT ( 'NONE', #3470 ) ;
#6067 = ORIENTED_EDGE ( 'NONE', *, *, #4055, .T. ) ;
#6068 = CARTESIAN_POINT ( 'NONE',  ( -4.143041610105385963, 4.340967609746959610, 12.11397738943082913 ) ) ;
#6069 = ORIENTED_EDGE ( 'NONE', *, *, #10113, .F. ) ;
#6070 = AXIS2_PLACEMENT_3D ( 'NONE', #3384, #7296, #9685 ) ;
#6071 = CARTESIAN_POINT ( 'NONE',  ( -2.066987299999999195, -0.8561741729129466183, 1.300000001092474600 ) ) ;
#6072 = CARTESIAN_POINT ( 'NONE',  ( 0.5031281619707679287, 5.980084330432668516, 4.126022727445257665 ) ) ;
#6073 = CARTESIAN_POINT ( 'NONE',  ( 5.903472034603481688, 2.056448723545244217, 32.00008219321556879 ) ) ;
#6074 = CARTESIAN_POINT ( 'NONE',  ( -0.8561741729129467293, 185.7999999989075093, 9.066987299999999195 ) ) ;
#6075 = CARTESIAN_POINT ( 'NONE',  ( -1.035533905932738197, -2.500000000000000000, 1.849999999999999867 ) ) ;
#6076 = CYLINDRICAL_SURFACE ( 'NONE', #4909, 1.999999999999999556 ) ;
#6077 = CARTESIAN_POINT ( 'NONE',  ( -0.8561741729129455081, 2.066987299999999639, -1.299999998907525267 ) ) ;
#6078 = DIRECTION ( 'NONE',  ( 0.8090169943749421222, 0.5877852522924802425, 0.000000000000000000 ) ) ;
#6079 = CARTESIAN_POINT ( 'NONE',  ( -0.9647310034392982958, 228.2043607281333379, 10.01900208526334168 ) ) ;
#6080 = CARTESIAN_POINT ( 'NONE',  ( 9.750000000000003553, 19.99999999999999645, 1.500000000000101696 ) ) ;
#6081 = VERTEX_POINT ( 'NONE', #4298 ) ;
#6082 = VECTOR ( 'NONE', #2415, 1000.000000000000000 ) ;
#6083 = ORIENTED_EDGE ( 'NONE', *, *, #9594, .F. ) ;
#6084 = CARTESIAN_POINT ( 'NONE',  ( 5.131373506000437068, 7.062729720844210135, 24.49999999999999289 ) ) ;
#6085 = ORIENTED_EDGE ( 'NONE', *, *, #635, .F. ) ;
#6086 = ORIENTED_EDGE ( 'NONE', *, *, #6435, .T. ) ;
#6087 = CARTESIAN_POINT ( 'NONE',  ( -6.176542424588090441, 0.9554180641287481901, 24.63234125634168237 ) ) ;
#6088 = CYLINDRICAL_SURFACE ( 'NONE', #5817, 1.000000000000000888 ) ;
#6089 = CARTESIAN_POINT ( 'NONE',  ( 0.8738043859790753931, -6.188821459035878547, 5.503415602237494042 ) ) ;
#6090 = CARTESIAN_POINT ( 'NONE',  ( -5.648559266344512331, -2.676764518775965218, 31.61396179408071916 ) ) ;
#6091 = LINE ( 'NONE', #12200, #7054 ) ;
#6092 = COLOUR_RGB ( '', 0.66274510, 0.83137255, 0.94901961) ;
#6093 = CARTESIAN_POINT ( 'NONE',  ( -0.7995524673973605223, -6.199337389817293875, 25.11453679452459298 ) ) ;
#6094 = CARTESIAN_POINT ( 'NONE',  ( -2.841519077896212497, 5.566940434249979752, 11.23620383159194347 ) ) ;
#6095 = CARTESIAN_POINT ( 'NONE',  ( 0.9735856429314211358, -5.920699391845005266, 18.26285283906725709 ) ) ;
#6096 = DIRECTION ( 'NONE',  ( 1.062480551894329468E-17, 3.608224830031754812E-16, -1.000000000000000000 ) ) ;
#6097 = DIRECTION ( 'NONE',  ( 0.000000000000000000, -1.000000000000000000, 0.000000000000000000 ) ) ;
#6098 = B_SPLINE_CURVE_WITH_KNOTS ( 'NONE', 3,
 ( #2394, #12099, #1198, #6072, #9733, #14571, #3030, #1514, #6390, #4061, #1669, #9012, #8931, #7568, #12650, #14890, #4299, #7645 ),
 .UNSPECIFIED., .F., .F.,
 ( 4, 2, 2, 2, 2, 2, 2, 2, 4 ),
 ( 0.003131923598876998338, 0.003523316383094315246, 0.003914709167311632154, 0.004306101951528949062, 0.004697494735746265970, 0.005088887519963582878, 0.005480280304180900654, 0.005871673088398217562, 0.006263065872615534470 ),
 .UNSPECIFIED. ) ;
#6099 = CARTESIAN_POINT ( 'NONE',  ( -1.035533905932737975, 188.9499999978150697, 4.500000000000000888 ) ) ;
#6100 = CARTESIAN_POINT ( 'NONE',  ( 2.899241599682305992, 227.5396000034540975, 8.063657412308430139 ) ) ;
#6101 = CARTESIAN_POINT ( 'NONE',  ( 5.329945432499600955, 2.755769831645193957, 11.23770962164069154 ) ) ;
#6102 = B_SPLINE_CURVE_WITH_KNOTS ( 'NONE', 3,
 ( #8746, #1406, #2927, #530, #8907, #376, #3950, #10248, #2687, #13504, #3873, #13653, #15099, #7622, #12466, #4195, #1568, #7466 ),
 .UNSPECIFIED., .F., .F.,
 ( 4, 2, 2, 2, 2, 2, 2, 2, 4 ),
 ( 0.000000000000000000, 0.0003914898357794970615, 0.0007829796715589941230, 0.001174469507338491130, 0.001565959343117988246, 0.001957449178897485362, 0.002348939014676982261, 0.002740428850456479593, 0.003131918686235976492 ),
 .UNSPECIFIED. ) ;
#6103 = EDGE_CURVE ( 'NONE', #13656, #10812, #9161, .T. ) ;
#6104 = CARTESIAN_POINT ( 'NONE',  ( 5.409423237178992316, 2.597448116731069234, 31.61561732698606164 ) ) ;
#6105 = MECHANICAL_DESIGN_GEOMETRIC_PRESENTATION_REPRESENTATION (  '', ( #9157 ), #6368 ) ;
#6106 = EDGE_LOOP ( 'NONE', ( #6613, #14584, #6945, #11934 ) ) ;
#6107 = CARTESIAN_POINT ( 'NONE',  ( -9.750000000000003553, 184.0000000000000000, 1.499999999999965583 ) ) ;
#6108 = AXIS2_PLACEMENT_3D ( 'NONE', #7601, #13487, #2832 ) ;
#6109 = CARTESIAN_POINT ( 'NONE',  ( -0.9999196734182004276, -5.916093360767527010, 11.36725955955069622 ) ) ;
#6110 = EDGE_CURVE ( 'NONE', #9644, #5984, #10193, .T. ) ;
#6111 = CARTESIAN_POINT ( 'NONE',  ( 5.317509234264027107, 2.779225709350867213, 24.49999999999999289 ) ) ;
#6112 = CARTESIAN_POINT ( 'NONE',  ( 2.817313151351169331, -5.579000502529441796, 31.00000000000000000 ) ) ;
#6113 = LINE ( 'NONE', #1315, #5122 ) ;
#6114 = CARTESIAN_POINT ( 'NONE',  ( -3.923477796648607185, 4.541042560386401306, 10.62696220972946826 ) ) ;
#6115 = EDGE_CURVE ( 'NONE', #660, #4645, #1314, .T. ) ;
#6116 = CARTESIAN_POINT ( 'NONE',  ( 0.8561741729129451750, 2.066987299999999639, -0.3999999989075250784 ) ) ;
#6117 = CARTESIAN_POINT ( 'NONE',  ( 9.750000000000003553, 22.00000000000000000, 1.020968533498575335E-13 ) ) ;
#6118 =( LENGTH_UNIT ( ) NAMED_UNIT ( * ) SI_UNIT ( .MILLI., .METRE. ) );
#6119 = AXIS2_PLACEMENT_3D ( 'NONE', #192, #4742, #13479 ) ;
#6120 = CARTESIAN_POINT ( 'NONE',  ( -5.984759433607008461, 1.806271833852296282, 12.50008219321554925 ) ) ;
#6121 = VECTOR ( 'NONE', #9447, 1000.000000000000000 ) ;
#6122 = CARTESIAN_POINT ( 'NONE',  ( -1.035533905932737753, 184.2500000000000000, 4.500000000000000888 ) ) ;
#6123 = DIRECTION ( 'NONE',  ( 1.000000000000000000, 0.000000000000000000, 0.000000000000000000 ) ) ;
#6124 = EDGE_CURVE ( 'NONE', #11937, #10357, #9718, .T. ) ;
#6125 = CARTESIAN_POINT ( 'NONE',  ( 1.078411626687468594, 228.8081072869749732, 8.573250792970148026 ) ) ;
#6126 = CARTESIAN_POINT ( 'NONE',  ( -0.8561741729129455081, 2.066987299999999639, 0.5000000010924748883 ) ) ;
#6127 = CARTESIAN_POINT ( 'NONE',  ( 2.082642335314403343E-14, 6.000000000000000888, 32.00000000000000000 ) ) ;
#6128 = ORIENTED_EDGE ( 'NONE', *, *, #9412, .T. ) ;
#6129 = CARTESIAN_POINT ( 'NONE',  ( 2.066987300000000083, 189.0999999989075206, 6.143825827087054492 ) ) ;
#6130 = CARTESIAN_POINT ( 'NONE',  ( 1.461580736456473240, 187.5499999989075093, 5.538419263543526760 ) ) ;
#6131 = CARTESIAN_POINT ( 'NONE',  ( -3.159082487394789585, -5.393634094348327856, 12.29954462468842458 ) ) ;
#6132 = EDGE_LOOP ( 'NONE', ( #7813, #9728 ) ) ;
#6133 = DIRECTION ( 'NONE',  ( 0.000000000000000000, 0.000000000000000000, -1.000000000000000000 ) ) ;
#6134 = DIRECTION ( 'NONE',  ( -6.123233995736766036E-17, 1.000000000000000000, 0.000000000000000000 ) ) ;
#6135 = EDGE_CURVE ( 'NONE', #6640, #13830, #12490, .T. ) ;
#6136 = CARTESIAN_POINT ( 'NONE',  ( -3.000000000000000000, 0.000000000000000000, 0.000000000000000000 ) ) ;
#6137 = CARTESIAN_POINT ( 'NONE',  ( 0.000000000000000000, 229.2449477060184222, 9.834870838912449287 ) ) ;
#6138 = CARTESIAN_POINT ( 'NONE',  ( -0.05280746222630467585, 189.0001365486126303, 9.499442212161147481 ) ) ;
#6139 = CARTESIAN_POINT ( 'NONE',  ( 3.011899281037514697, -5.190111395030220010, 30.19977782616120621 ) ) ;
#6140 = CARTESIAN_POINT ( 'NONE',  ( -0.1306171417088389242, -6.000000000000001776, 30.00000000000000000 ) ) ;
#6141 = CARTESIAN_POINT ( 'NONE',  ( 5.317509234263979145, -2.779225709350955142, 31.00000000000000000 ) ) ;
#6142 = DIRECTION ( 'NONE',  ( -0.8660254037844385966, 0.5000000000000001110, 0.000000000000000000 ) ) ;
#6143 = CARTESIAN_POINT ( 'NONE',  ( 5.317509234263932072, 2.779225709351047957, 5.000000000000004441 ) ) ;
#6144 = CARTESIAN_POINT ( 'NONE',  ( -2.500000000000000888, 187.5999999999999943, 7.000000000000000000 ) ) ;
#6145 = ORIENTED_EDGE ( 'NONE', *, *, #1759, .F. ) ;
#6146 = EDGE_CURVE ( 'NONE', #1465, #14884, #14450, .T. ) ;
#6147 = ORIENTED_EDGE ( 'NONE', *, *, #11241, .F. ) ;
#6148 = ORIENTED_EDGE ( 'NONE', *, *, #9503, .F. ) ;
#6149 = CARTESIAN_POINT ( 'NONE',  ( -4.286401442266736694, 4.198423832312983883, 24.63064961348855775 ) ) ;
#6150 = EDGE_CURVE ( 'NONE', #8455, #5900, #3783, .T. ) ;
#6151 = EDGE_LOOP ( 'NONE', ( #9273, #1194 ) ) ;
#6152 = CARTESIAN_POINT ( 'NONE',  ( -1.265664690411614835E-16, 2.066987299999999639, 1.850000001092474644 ) ) ;
#6153 = CYLINDRICAL_SURFACE ( 'NONE', #10864, 2.500000000000000444 ) ;
#6154 = CARTESIAN_POINT ( 'NONE',  ( 2.500000000000000444, 1.035533905932737975, -0.2500000000000002220 ) ) ;
#6155 = CARTESIAN_POINT ( 'NONE',  ( -1.461580736456473018, 187.9499999989075150, 5.538419263543527649 ) ) ;
#6156 = CARTESIAN_POINT ( 'NONE',  ( -1.035533905932738197, -2.500000000000000000, 1.050000000000000044 ) ) ;
#6157 = CARTESIAN_POINT ( 'NONE',  ( -5.935543223013858949, 0.8771126767606857166, 31.00000000000000000 ) ) ;
#6158 = CONTEXT_DEPENDENT_SHAPE_REPRESENTATION ( #7410, #8194 ) ;
#6159 = DIRECTION ( 'NONE',  ( 0.5877852522924802425, -0.8090169943749422332, 0.000000000000000000 ) ) ;
#6160 = CARTESIAN_POINT ( 'NONE',  ( -1.461580736456472795, 1.461580736456472795, -2.049999998907525711 ) ) ;
#6161 = CARTESIAN_POINT ( 'NONE',  ( 3.883716939929134693, -4.898343590941131254, 30.02640428276698970 ) ) ;
#6162 = CARTESIAN_POINT ( 'NONE',  ( -2.998822209637060254, 227.3208645008386668, 7.419865387590665939 ) ) ;
#6163 = CARTESIAN_POINT ( 'NONE',  ( 5.616116467183593919, 2.743044348085676987, 5.504259495030093596 ) ) ;
#6164 = ORIENTED_EDGE ( 'NONE', *, *, #14946, .T. ) ;
#6165 = CIRCLE ( 'NONE', #9960, 7.000000000000000000 ) ;
#6166 = ORIENTED_EDGE ( 'NONE', *, *, #11434, .F. ) ;
#6167 = EDGE_CURVE ( 'NONE', #15370, #4806, #3731, .T. ) ;
#6168 = ORIENTED_EDGE ( 'NONE', *, *, #5940, .F. ) ;
#6169 = CARTESIAN_POINT ( 'NONE',  ( -5.570820891630755334, -2.833901239560420837, 11.23763026556121858 ) ) ;
#6170 = LINE ( 'NONE', #7661, #10378 ) ;
#6171 = CARTESIAN_POINT ( 'NONE',  ( -2.849573632035356852, -5.280958870664559157, 25.11561732698605098 ) ) ;
#6172 = CARTESIAN_POINT ( 'NONE',  ( 2.782156709077431067, -5.316215864844039629, 12.00312048902376993 ) ) ;
#6173 = UNCERTAINTY_MEASURE_WITH_UNIT (LENGTH_MEASURE( 1.000000000000000082E-05 ), #14055, 'distance_accuracy_value', 'NONE');
#6174 = CARTESIAN_POINT ( 'NONE',  ( 4.153663429050693523, -4.670992970568449643, 23.70066851092423832 ) ) ;
#6175 = CARTESIAN_POINT ( 'NONE',  ( -4.286401442266580375, -4.198423832313147308, 11.63061695532136852 ) ) ;
#6176 = CARTESIAN_POINT ( 'NONE',  ( 5.375886393124412521, -2.665038680141230909, 12.00439760644213294 ) ) ;
#6177 = CARTESIAN_POINT ( 'NONE',  ( 0.8736516769108282343, -5.936271176698213914, 17.49606771578676856 ) ) ;
#6178 = CARTESIAN_POINT ( 'NONE',  ( -2.500000000000000444, 188.3499999999999943, 5.964466094067261359 ) ) ;
#6179 = DIRECTION ( 'NONE',  ( 0.000000000000000000, -1.000000000000000000, 0.000000000000000000 ) ) ;
#6180 = CARTESIAN_POINT ( 'NONE',  ( 1.035533905932738197, 188.5499999978150356, 9.500000000000003553 ) ) ;
#6181 = CARTESIAN_POINT ( 'NONE',  ( 2.692585213447247661, 226.8629897650803855, 6.071564533969844746 ) ) ;
#6182 = CARTESIAN_POINT ( 'NONE',  ( 5.935543223013858061, 0.8771126767606804986, 11.36935038651144581 ) ) ;
#6183 = CARTESIAN_POINT ( 'NONE',  ( -1.503949710467194167, 189.0000000002120260, 9.002347884774902553 ) ) ;
#6184 = AXIS2_PLACEMENT_3D ( 'NONE', #10468, #992, #8321 ) ;
#6185 = ORIENTED_EDGE ( 'NONE', *, *, #7306, .T. ) ;
#6186 = CARTESIAN_POINT ( 'NONE',  ( -3.312341048453451009, 5.004306261885466789, 4.026019798777604741 ) ) ;
#6187 =( REPRESENTATION_RELATIONSHIP ('NONE','NONE', #11191, #8978 ) REPRESENTATION_RELATIONSHIP_WITH_TRANSFORMATION ( #4326 )SHAPE_REPRESENTATION_RELATIONSHIP( ) );
#6188 = CARTESIAN_POINT ( 'NONE',  ( 6.768587589771821120E-14, -6.000000000000000888, 12.49999999999998401 ) ) ;
#6189 = DIRECTION ( 'NONE',  ( 0.000000000000000000, 0.000000000000000000, -1.000000000000000000 ) ) ;
#6190 = CARTESIAN_POINT ( 'NONE',  ( 2.031800924177950305E-13, 6.000000000000000888, 23.49999999999999289 ) ) ;
#6191 = CARTESIAN_POINT ( 'NONE',  ( 0.9637716067245765128, 226.3761301684456555, 4.636858967466513270 ) ) ;
#6192 = DIRECTION ( 'NONE',  ( -0.9510565162951544194, 0.3090169943749447312, 0.000000000000000000 ) ) ;
#6193 = EDGE_CURVE ( 'NONE', #12811, #2830, #13589, .T. ) ;
#6194 = CARTESIAN_POINT ( 'NONE',  ( -2.066987299999999639, 0.000000000000000000, 0.6500000010924747995 ) ) ;
#6195 = CARTESIAN_POINT ( 'NONE',  ( 5.330189595673641811, -2.755293208590234411, 4.736173967944048435 ) ) ;
#6196 = VECTOR ( 'NONE', #1, 1000.000000000000000 ) ;
#6197 = CARTESIAN_POINT ( 'NONE',  ( -3.000000000000000444, -1.732050807568878081, -5.500000000000000000 ) ) ;
#6198 = CARTESIAN_POINT ( 'NONE',  ( -1.490777987167568597E-16, 188.9300000002185129, 4.500000000000000000 ) ) ;
#6199 = CARTESIAN_POINT ( 'NONE',  ( 0.000000000000000000, 0.000000000000000000, 53.67766952966368876 ) ) ;
#6200 = CARTESIAN_POINT ( 'NONE',  ( 0.2588337889006175341, 228.9066910274044346, 8.857966258178848307 ) ) ;
#6201 = DIRECTION ( 'NONE',  ( -0.000000000000000000, 1.000000000000000000, -0.000000000000000000 ) ) ;
#6202 = CARTESIAN_POINT ( 'NONE',  ( 6.172651332693102511, 0.9815532474593232637, 17.73809786915987274 ) ) ;
#6203 = ORIENTED_EDGE ( 'NONE', *, *, #4688, .T. ) ;
#6204 = CARTESIAN_POINT ( 'NONE',  ( -1.461580736456472351, -1.461580736456473018, 1.350000001092474644 ) ) ;
#6205 = CARTESIAN_POINT ( 'NONE',  ( -2.066987300000000971, 186.1999999989075150, 6.143825827087054492 ) ) ;
#6206 = CARTESIAN_POINT ( 'NONE',  ( 5.620786884546339124, 2.102685372472758552, 23.52641404563304661 ) ) ;
#6208 = EDGE_LOOP ( 'NONE', ( #9506, #5695 ) ) ;
#6207 = CARTESIAN_POINT ( 'NONE',  ( 3.253823204785117440, 5.337590213880504919, 30.12694108445699825 ) ) ;
#6209 = VECTOR ( 'NONE', #2108, 1000.000000000000000 ) ;
#6210 =( LENGTH_UNIT ( ) NAMED_UNIT ( * ) SI_UNIT ( .MILLI., .METRE. ) );
#6211 = EDGE_CURVE ( 'NONE', #11236, #5801, #9773, .T. ) ;
#6212 = CARTESIAN_POINT ( 'NONE',  ( 0.8002720181892983842, -6.199262377003380564, 23.88606262465556185 ) ) ;
#6213 = ADVANCED_FACE ( 'NONE', ( #3707 ), #8584, .F. ) ;
#6214 = SURFACE_SIDE_STYLE ('',( #11128 ) ) ;
#6215 = CARTESIAN_POINT ( 'NONE',  ( 5.999999999999999112, 202.3202208672780102, 7.308763624231163547 ) ) ;
#6216 = CARTESIAN_POINT ( 'NONE',  ( -2.108001641305449425, 189.0000000000000284, 8.365019857495370914 ) ) ;
#6217 = CARTESIAN_POINT ( 'NONE',  ( -1.035533905932738197, -2.500000000000000000, 0.2499999999999997780 ) ) ;
#6218 = DIRECTION ( 'NONE',  ( 1.000000000000000000, 0.000000000000000000, 0.000000000000000000 ) ) ;
#6219 = CARTESIAN_POINT ( 'NONE',  ( -0.6144377077729746839, -5.969178481556069116, 30.20033966857736729 ) ) ;
#6220 =( BOUNDED_CURVE ( )  B_SPLINE_CURVE ( 2, ( #9929, #9778, #6438, #6274, #3942, #13736, #2681, #9851, #134 ),
 .UNSPECIFIED., .F., .F. ) 
 B_SPLINE_CURVE_WITH_KNOTS ( ( 3, 2, 2, 2, 3 ),
 ( 0.6428571428571429047, 0.6607142857142856984, 0.6785714285714286031, 0.6964285714285713969, 0.7142857142857143016 ),
 .UNSPECIFIED. ) 
 CURVE ( )  GEOMETRIC_REPRESENTATION_ITEM ( )  RATIONAL_B_SPLINE_CURVE ( ( 1.000000000000000000, 0.9238795325112867385, 1.000000000000000000, 0.9238795325112867385, 1.000000000000000000, 0.9238795325112867385, 1.000000000000000000, 0.9238795325112867385, 1.000000000000000000 ) ) 
 REPRESENTATION_ITEM ( '' )  );
#6221 = CARTESIAN_POINT ( 'NONE',  ( -2.500000000000000444, 184.3499999999999943, 5.964466094067261359 ) ) ;
#6222 = CARTESIAN_POINT ( 'NONE',  ( -5.783239563508424830, 1.602707436861116497, 10.52641404563305194 ) ) ;
#6223 = CARTESIAN_POINT ( 'NONE',  ( -6.081464507797636365, 1.446657058464182022, 10.62619944752603018 ) ) ;
#6224 = CARTESIAN_POINT ( 'NONE',  ( 3.419318284370060912, 4.932111238568271716, 23.50007997643737312 ) ) ;
#6225 = ORIENTED_EDGE ( 'NONE', *, *, #275, .F. ) ;
#6226 = EDGE_LOOP ( 'NONE', ( #11301, #9563, #3057, #3446 ) ) ;
#6227 = AXIS2_PLACEMENT_3D ( 'NONE', #9435, #9280, #14267 ) ;
#6228 = EDGE_LOOP ( 'NONE', ( #11720, #10867, #14671, #13989 ) ) ;
#6229 = DIRECTION ( 'NONE',  ( 0.000000000000000000, 0.000000000000000000, 1.000000000000000000 ) ) ;
#6230 = ORIENTED_EDGE ( 'NONE', *, *, #1802, .F. ) ;
#6231 = CARTESIAN_POINT ( 'NONE',  ( 1.461580736456473018, -1.461580736456472573, -0.8499999989075254225 ) ) ;
#6232 = DIRECTION ( 'NONE',  ( -0.000000000000000000, 1.000000000000000000, -0.000000000000000000 ) ) ;
#6233 = LINE ( 'NONE', #10756, #9729 ) ;
#6234 = CARTESIAN_POINT ( 'NONE',  ( 2.066987299999999195, 189.1999999989075434, 7.856174172912946396 ) ) ;
#6235 = CARTESIAN_POINT ( 'NONE',  ( 4.592425496802573972E-16, -2.500000000000000000, -2.093000000021849605 ) ) ;
#6236 =( BOUNDED_CURVE ( )  B_SPLINE_CURVE ( 2, ( #7117, #15391, #10609, #2163, #4809, #10688, #2409, #7197, #6000 ),
 .UNSPECIFIED., .F., .F. ) 
 B_SPLINE_CURVE_WITH_KNOTS ( ( 3, 2, 2, 2, 3 ),
 ( 0.2142857142857142738, 0.2321428571428571508, 0.2500000000000000000, 0.2678571428571428492, 0.2857142857142856984 ),
 .UNSPECIFIED. ) 
 CURVE ( )  GEOMETRIC_REPRESENTATION_ITEM ( )  RATIONAL_B_SPLINE_CURVE ( ( 1.000000000000000000, 0.9238795325112867385, 1.000000000000000000, 0.9238795325112867385, 1.000000000000000000, 0.9238795325112867385, 1.000000000000000000, 0.9238795325112867385, 1.000000000000000000 ) ) 
 REPRESENTATION_ITEM ( '' )  );
#6237 = CARTESIAN_POINT ( 'NONE',  ( -5.620879908643987122, 2.102487719021844281, 31.97377823943293151 ) ) ;
#6238 = CARTESIAN_POINT ( 'NONE',  ( 4.141923667210698490, -4.342011609040415721, 31.61561732698606875 ) ) ;
#6239 = CARTESIAN_POINT ( 'NONE',  ( 2.066987299999999639, 2.531329380823229670E-16, -1.549999998907525489 ) ) ;
#6240 = CARTESIAN_POINT ( 'NONE',  ( -6.176542424588117086, 0.9554180641285661135, 30.86762589283693359 ) ) ;
#6241 = CARTESIAN_POINT ( 'NONE',  ( -1.865818183961493126, 226.5341093703536899, 5.102530190813160615 ) ) ;
#6242 = ORIENTED_EDGE ( 'NONE', *, *, #4228, .F. ) ;
#6243 = ORIENTED_EDGE ( 'NONE', *, *, #7106, .T. ) ;
#6244 = ORIENTED_EDGE ( 'NONE', *, *, #12935, .F. ) ;
#6245 =( BOUNDED_CURVE ( )  B_SPLINE_CURVE ( 2, ( #14572, #9566, #8622, #8382, #9809, #3669, #14658, #6154, #8546 ),
 .UNSPECIFIED., .F., .F. ) 
 B_SPLINE_CURVE_WITH_KNOTS ( ( 3, 2, 2, 2, 3 ),
 ( 0.4285714285714285476, 0.4464285714285714524, 0.4642857142857143016, 0.4821428571428571508, 0.5000000000000000000 ),
 .UNSPECIFIED. ) 
 CURVE ( )  GEOMETRIC_REPRESENTATION_ITEM ( )  RATIONAL_B_SPLINE_CURVE ( ( 1.000000000000000000, 0.9238795325112867385, 1.000000000000000000, 0.9238795325112867385, 1.000000000000000000, 0.9238795325112867385, 1.000000000000000000, 0.9238795325112867385, 1.000000000000000000 ) ) 
 REPRESENTATION_ITEM ( '' )  );
#6246 = CARTESIAN_POINT ( 'NONE',  ( -7.490007020835642848, -2.433650805992559896, 24.49999999999999289 ) ) ;
#6247 = CARTESIAN_POINT ( 'NONE',  ( 2.471008581483269850, 189.0000000000000284, 6.581706670152065008 ) ) ;
#6248 = CIRCLE ( 'NONE', #1661, 2.500000000000000444 ) ;
#6249 = CARTESIAN_POINT ( 'NONE',  ( -0.8738118504725720381, -5.936246475285030577, 5.503572421742426890 ) ) ;
#6250 = CARTESIAN_POINT ( 'NONE',  ( -3.312341048453484316, -5.004306261885444584, 18.97398020122238904 ) ) ;
#6251 = CARTESIAN_POINT ( 'NONE',  ( 0.7988914244718910984, 5.947301735519275212, 10.88456289168616742 ) ) ;
#6252 = PLANE ( 'NONE',  #10221 ) ;
#6253 = EDGE_CURVE ( 'NONE', #10136, #7716, #13259, .T. ) ;
#6254 = FACE_OUTER_BOUND ( 'NONE', #8131, .T. ) ;
#6255 = CARTESIAN_POINT ( 'NONE',  ( -6.021167129161060672, -1.680051667990286601, 5.973595717233013858 ) ) ;
#6256 = CARTESIAN_POINT ( 'NONE',  ( 0.5039079366034465712, -5.980031194523134808, 23.62637068109812333 ) ) ;
#6257 = DIRECTION ( 'NONE',  ( 1.000000000000000000, 0.000000000000000000, 0.000000000000000000 ) ) ;
#6258 = CARTESIAN_POINT ( 'NONE',  ( -1.035533905932737753, 185.0199999975965284, 4.500000000000000888 ) ) ;
#6259 = CARTESIAN_POINT ( 'NONE',  ( -1.159640499634989608, 227.7308148186401979, 5.461968699681960082 ) ) ;
#6260 = CARTESIAN_POINT ( 'NONE',  ( 0.7798766585422360897, 226.3581810736479270, 4.583957619654694504 ) ) ;
#6261 = CARTESIAN_POINT ( 'NONE',  ( -0.05280792143845292053, 189.0000000000001137, 9.499442202459045248 ) ) ;
#6262 = ORIENTED_EDGE ( 'NONE', *, *, #6150, .T. ) ;
#6263 = DIRECTION ( 'NONE',  ( -0.000000000000000000, 1.000000000000000000, -0.000000000000000000 ) ) ;
#6264 = CARTESIAN_POINT ( 'NONE',  ( 6.780834054130108014E-14, -6.250000000000000888, 10.49999999999998224 ) ) ;
#6265 = CARTESIAN_POINT ( 'NONE',  ( 5.843318061569079624, 1.367618216965494238, 25.37303779027051576 ) ) ;
#6266 = CARTESIAN_POINT ( 'NONE',  ( 5.770288754215121330, 2.404361317819969646, 12.37381964045070504 ) ) ;
#6267 = CARTESIAN_POINT ( 'NONE',  ( 2.115286944722794438, 226.6055634003047032, 5.313108787231142216 ) ) ;
#6268 = CARTESIAN_POINT ( 'NONE',  ( 7.000000000000006217, 5.005650134388747156E-16, -1.500000000000000000 ) ) ;
#6269 = CARTESIAN_POINT ( 'NONE',  ( -2.066987299999999639, 0.000000000000000000, -1.749999998907525223 ) ) ;
#6270 = CARTESIAN_POINT ( 'NONE',  ( 4.435347140101010055, 4.403429997944536822, 5.000000000000004441 ) ) ;
#6271 =( NAMED_UNIT ( * ) SI_UNIT ( $, .STERADIAN. ) SOLID_ANGLE_UNIT ( ) );
#6272 = DIRECTION ( 'NONE',  ( 0.000000000000000000, 0.000000000000000000, 1.000000000000000000 ) ) ;
#6273 = CARTESIAN_POINT ( 'NONE',  ( -2.500000000000000444, 186.6800000002185413, 5.964466094067261359 ) ) ;
#6274 = CARTESIAN_POINT ( 'NONE',  ( 1.035533905932739085, -2.500000000000000000, -1.949999997815050401 ) ) ;
#6275 = CARTESIAN_POINT ( 'NONE',  ( 1.579185070784824285, 228.6572036374857078, 8.137432446265082220 ) ) ;
#6276 = CARTESIAN_POINT ( 'NONE',  ( 0.000000000000000000, 184.0000000000000000, 7.000000000000000000 ) ) ;
#6277 = CARTESIAN_POINT ( 'NONE',  ( 2.500000000000000444, 1.035533905932737975, -2.549999997815050712 ) ) ;
#6278 = VERTEX_POINT ( 'NONE', #8660 ) ;
#6279 = CARTESIAN_POINT ( 'NONE',  ( -2.066987299999999639, 0.8561741729129455081, 0.4000000010924748550 ) ) ;
#6280 = CARTESIAN_POINT ( 'NONE',  ( 2.500000000000000444, 185.5500000000000114, 8.035533905932739529 ) ) ;
#6281 = CARTESIAN_POINT ( 'NONE',  ( 5.984377695197274249, -1.807429553002113609, 19.00004906876531408 ) ) ;
#6283 = ORIENTED_EDGE ( 'NONE', *, *, #11, .T. ) ;
#6282 = CARTESIAN_POINT ( 'NONE',  ( -2.066987300000000527, 184.8999999989075320, 7.856174172912944620 ) ) ;
#6284 = CARTESIAN_POINT ( 'NONE',  ( -3.107688324358802490, -5.133887830459779700, 23.62621569129737864 ) ) ;
#6285 = CARTESIAN_POINT ( 'NONE',  ( 6.176542424588128632, -0.9554180641284775177, 11.49999999999998224 ) ) ;
#6286 = CARTESIAN_POINT ( 'NONE',  ( 2.500000000000000000, 3.061616997868383141E-16, -1.100000000000000311 ) ) ;
#6287 = AXIS2_PLACEMENT_3D ( 'NONE', #1169, #10883, #3475 ) ;
#6288 = CARTESIAN_POINT ( 'NONE',  ( 0.6144300524834573896, 6.220417338033042753, 10.70033372175934439 ) ) ;
#6289 = CARTESIAN_POINT ( 'NONE',  ( -1.967615029119349934, 189.0000000000000284, 5.432308397871834060 ) ) ;
#6290 = FACE_OUTER_BOUND ( 'NONE', #6151, .T. ) ;
#6291 = CARTESIAN_POINT ( 'NONE',  ( 1.035533905932739085, -2.500000000000000000, -1.949999997815050401 ) ) ;
#6292 = FACE_OUTER_BOUND ( 'NONE', #14066, .T. ) ;
#6293 = CARTESIAN_POINT ( 'NONE',  ( 5.330189595673669345, -2.755293208590180232, 11.23617396794405288 ) ) ;
#6294 = CARTESIAN_POINT ( 'NONE',  ( -0.7988860301920965856, -6.199427171881353615, 17.38455580536194489 ) ) ;
#6295 = DIRECTION ( 'NONE',  ( 0.000000000000000000, 0.000000000000000000, -1.000000000000000000 ) ) ;
#6296 = CARTESIAN_POINT ( 'NONE',  ( -5.317509234263959605, 2.779225709350992002, 31.00000000000000000 ) ) ;
#6297 = EDGE_CURVE ( 'NONE', #14222, #13893, #14797, .T. ) ;
#6298 = VERTEX_POINT ( 'NONE', #6268 ) ;
#6299 = CARTESIAN_POINT ( 'NONE',  ( 2.066987299999999195, 188.3999999989075036, 7.856174172912946396 ) ) ;
#6300 = PRODUCT_DEFINITION_FORMATION_WITH_SPECIFIED_SOURCE ( 'ANY', '', #4768, .NOT_KNOWN. ) ;
#6301 = EDGE_CURVE ( 'NONE', #1760, #5982, #15688, .T. ) ;
#6302 = ORIENTED_EDGE ( 'NONE', *, *, #10587, .F. ) ;
#6303 = AXIS2_PLACEMENT_3D ( 'NONE', #1491, #1726, #13819 ) ;
#6304 = ORIENTED_EDGE ( 'NONE', *, *, #13392, .F. ) ;
#6305 = CARTESIAN_POINT ( 'NONE',  ( -4.196038884587333762, 4.289036423669111642, 25.00389795015983552 ) ) ;
#6306 = ADVANCED_FACE ( 'NONE', ( #6432 ), #13959, .F. ) ;
#6307 = VERTEX_POINT ( 'NONE', #6583 ) ;
#6308 = CARTESIAN_POINT ( 'NONE',  ( 2.066987300000000083, -0.8561741729129449530, 1.092474635061568626E-09 ) ) ;
#6309 = CARTESIAN_POINT ( 'NONE',  ( 0.000000000000000000, 2.000000000000000000, -20.00000000000000000 ) ) ;
#6310 = AXIS2_PLACEMENT_3D ( 'NONE', #2685, #13502, #8670 ) ;
#6311 = CARTESIAN_POINT ( 'NONE',  ( -2.103459429923432822, 227.9779199259797622, 9.353140775971661824 ) ) ;
#6312 = DIRECTION ( 'NONE',  ( 0.000000000000000000, 0.000000000000000000, -1.000000000000000000 ) ) ;
#6313 = CARTESIAN_POINT ( 'NONE',  ( -1.035533905932737753, 2.500000000000000444, -2.443000000021850138 ) ) ;
#6314 = VECTOR ( 'NONE', #9240, 1000.000000000000000 ) ;
#6315 = CARTESIAN_POINT ( 'NONE',  ( -5.486741141153809842, 2.429871531109698335, 31.79888242247943353 ) ) ;
#6316 = FACE_OUTER_BOUND ( 'NONE', #11467, .T. ) ;
#6317 = CARTESIAN_POINT ( 'NONE',  ( 1.461580736456472573, 1.461580736456472795, 0.3500000010924749216 ) ) ;
#6318 = CARTESIAN_POINT ( 'NONE',  ( -6.176542424588117974, 0.9554180641285661135, 31.00000000000000000 ) ) ;
#6319 = CARTESIAN_POINT ( 'NONE',  ( -2.257704606524308488, 227.9260547655458140, 9.200601119324863575 ) ) ;
#6320 = EDGE_CURVE ( 'NONE', #6066, #3385, #2990, .T. ) ;
#6321 = ORIENTED_EDGE ( 'NONE', *, *, #11273, .T. ) ;
#6322 = EDGE_LOOP ( 'NONE', ( #5906, #7118, #7811, #3388 ) ) ;
#6323 = ORIENTED_EDGE ( 'NONE', *, *, #968, .T. ) ;
#6324 = CYLINDRICAL_SURFACE ( 'NONE', #13337, 1.000000000000000888 ) ;
#6325 = CARTESIAN_POINT ( 'NONE',  ( 2.930600586412970276, 5.520563544161749547, 4.496913561339538568 ) ) ;
#6326 = EDGE_LOOP ( 'NONE', ( #4611, #8516, #5494, #8336 ) ) ;
#6327 = CARTESIAN_POINT ( 'NONE',  ( 0.6144300524833581356, 6.220417338033051635, 4.200333721759339944 ) ) ;
#6328 =( BOUNDED_CURVE ( )  B_SPLINE_CURVE ( 2, ( #3499, #10821, #953, #9393, #12963, #14231, #13285, #9639, #5820 ),
 .UNSPECIFIED., .F., .F. ) 
 B_SPLINE_CURVE_WITH_KNOTS ( ( 3, 2, 2, 2, 3 ),
 ( 0.2857142857142856984, 0.3035714285714285476, 0.3214285714285714524, 0.3392857142857143016, 0.3571428571428571508 ),
 .UNSPECIFIED. ) 
 CURVE ( )  GEOMETRIC_REPRESENTATION_ITEM ( )  RATIONAL_B_SPLINE_CURVE ( ( 1.000000000000000000, 0.9238795325112867385, 1.000000000000000000, 0.9238795325112867385, 1.000000000000000000, 0.9238795325112867385, 1.000000000000000000, 0.9238795325112867385, 1.000000000000000000 ) ) 
 REPRESENTATION_ITEM ( '' )  );
#6329 = CARTESIAN_POINT ( 'NONE',  ( 0.8002720181892442053, -6.199262377003387670, 17.38606262465557606 ) ) ;
#6330 = CARTESIAN_POINT ( 'NONE',  ( 3.568242062701445949, -5.132954954975562423, 23.49995093123466461 ) ) ;
#6331 = CARTESIAN_POINT ( 'NONE',  ( -1.767766952966369320, 187.3999999978150584, 5.232233047033630235 ) ) ;
#6332 = CARTESIAN_POINT ( 'NONE',  ( -1.035533905932737753, 185.0499999999999829, 4.500000000000001776 ) ) ;
#6333 = CARTESIAN_POINT ( 'NONE',  ( 5.843075991566598404, -1.368655265450984704, 12.37364704684421035 ) ) ;
#6334 = CARTESIAN_POINT ( 'NONE',  ( -3.158825713737648755, 5.393784879207071725, 18.79933148907576168 ) ) ;
#6335 = APPLICATION_PROTOCOL_DEFINITION ( 'draft international standard', 'automotive_design', 1998, #8009 ) ;
#6336 = VECTOR ( 'NONE', #14442, 1000.000000000000000 ) ;
#6337 = CARTESIAN_POINT ( 'NONE',  ( 2.500000000000000444, 184.8199999975965682, 5.964466094067262247 ) ) ;
#6338 = CARTESIAN_POINT ( 'NONE',  ( -1.984331290054332841, 228.3135221411288285, 7.144860682478253011 ) ) ;
#6339 = CARTESIAN_POINT ( 'NONE',  ( -2.599074790483714370, 227.7726799100639994, 8.749447567440038043 ) ) ;
#6340 = CARTESIAN_POINT ( 'NONE',  ( -2.521737919408184148, 188.9999999974891409, 6.973570937152097748 ) ) ;
#6341 = EDGE_CURVE ( 'NONE', #13293, #4150, #11898, .T. ) ;
#6342 = ORIENTED_EDGE ( 'NONE', *, *, #10406, .T. ) ;
#6343 = CARTESIAN_POINT ( 'NONE',  ( -5.859221468178952286, 2.178708437343215731, 17.02591457665827690 ) ) ;
#6344 = B_SPLINE_CURVE_WITH_KNOTS ( 'NONE', 3,
 ( #8154, #9046, #4489, #10382, #10305, #4253, #14184, #5459, #11722, #3290, #747, #2091, #10460, #4416, #1860, #5613, #15233, #9269 ),
 .UNSPECIFIED., .F., .F.,
 ( 4, 2, 2, 2, 2, 2, 2, 2, 4 ),
 ( 0.000000000000000000, 0.0003914362731607522075, 0.0007828725463215044150, 0.001174308819482256568, 0.001565745092643008830, 0.001957181365803761092, 0.002348617638964513137, 0.002740053912125265615, 0.003131490185286017660 ),
 .UNSPECIFIED. ) ;
#6345 = CARTESIAN_POINT ( 'NONE',  ( 3.254737477228021536, -5.337033878705195633, 10.62632671364005432 ) ) ;
#6346 = PRODUCT_DEFINITION ( 'UNKNOWN', '', #2733, #526 ) ;
#6347 = CARTESIAN_POINT ( 'NONE',  ( -4.006441409774867957, 4.467329318258094872, 23.70111757752058068 ) ) ;
#6348 = CARTESIAN_POINT ( 'NONE',  ( 0.8730424326982959560, 5.936362132114433976, 23.99500690218563648 ) ) ;
#6349 = AXIS2_PLACEMENT_3D ( 'NONE', #15513, #3405, #8197 ) ;
#6350 = CARTESIAN_POINT ( 'NONE',  ( 2.688173913331684428, 227.7236097417891187, 8.605093950198996922 ) ) ;
#6351 = EDGE_CURVE ( 'NONE', #7562, #7176, #15321, .T. ) ;
#6352 = CARTESIAN_POINT ( 'NONE',  ( -2.817313151351126255, -5.579000502529464889, 31.13234125634170368 ) ) ;
#6353 = CARTESIAN_POINT ( 'NONE',  ( -1.530808498934191571E-16, 2.500000000000000000, 1.500000000000000000 ) ) ;
#6354 = CARTESIAN_POINT ( 'NONE',  ( -3.781065399486156497, 4.978303713186331692, 23.50008258189710020 ) ) ;
#6355 = CARTESIAN_POINT ( 'NONE',  ( 5.843318061569033439, 1.367618216965686972, 5.873037790270514868 ) ) ;
#6356 = CARTESIAN_POINT ( 'NONE',  ( -6.776263578034402713E-18, 186.5999999999999943, 4.500000000000000000 ) ) ;
#6357 = DIRECTION ( 'NONE',  ( -6.123233995736766036E-17, 1.000000000000000000, 0.000000000000000000 ) ) ;
#6358 = CARTESIAN_POINT ( 'NONE',  ( 1.211961328308884367, 228.7773363860045492, 8.484382675910040916 ) ) ;
#6359 = CARTESIAN_POINT ( 'NONE',  ( -1.461580736456472795, 1.461580736456472795, -1.849999998907525534 ) ) ;
#6360 = CARTESIAN_POINT ( 'NONE',  ( 3.159612573729187357, 5.393342049074656863, 12.30026515017674882 ) ) ;
#6361 = AXIS2_PLACEMENT_3D ( 'NONE', #5692, #10537, #6657 ) ;
#6362 = CARTESIAN_POINT ( 'NONE',  ( 1.461580736456472573, 1.461580736456472795, 0.1500000010924747995 ) ) ;
#6363 = CARTESIAN_POINT ( 'NONE',  ( -2.066987300000001415, 188.5999999989074922, 6.143825827087054492 ) ) ;
#6364 = CARTESIAN_POINT ( 'NONE',  ( -3.420659742068490328, 4.931142898501661875, 18.99995053646221521 ) ) ;
#6366 = ORIENTED_EDGE ( 'NONE', *, *, #2340, .F. ) ;
#6365 = CARTESIAN_POINT ( 'NONE',  ( 0.8561741729129455081, 187.7999999989075093, 4.933012699999999029 ) ) ;
#6367 = CARTESIAN_POINT ( 'NONE',  ( -4.435347140101107755, -4.403429997944436458, 17.99999999999998934 ) ) ;
#6368 =( GEOMETRIC_REPRESENTATION_CONTEXT ( 3 ) GLOBAL_UNCERTAINTY_ASSIGNED_CONTEXT ( ( #14429 ) ) GLOBAL_UNIT_ASSIGNED_CONTEXT ( ( #6034, #1165, #6271 ) ) REPRESENTATION_CONTEXT ( 'NONE', 'WORKASPACE' ) );
#6369 = CARTESIAN_POINT ( 'NONE',  ( 5.616089948629760187, -2.743103014345478652, 12.00436969680152721 ) ) ;
#6370 = SURFACE_STYLE_USAGE ( .BOTH. , #11418 ) ;
#6371 = CARTESIAN_POINT ( 'NONE',  ( -5.666074146198027961, 1.978051345703067065, 3.999950679266886855 ) ) ;
#6372 = CARTESIAN_POINT ( 'NONE',  ( -0.2637975869347151114, -6.245592211692898132, 12.47332839949189598 ) ) ;
#6373 = CARTESIAN_POINT ( 'NONE',  ( 5.931828553038004159, -0.9033193133617308801, 24.76194324003146008 ) ) ;
#6374 = CARTESIAN_POINT ( 'NONE',  ( 1.973460340353461850, 189.7555967275478963, 9.640314175604393299 ) ) ;
#6375 = DIRECTION ( 'NONE',  ( -0.5877852522924685852, -0.8090169943749508930, 0.000000000000000000 ) ) ;
#6376 = CARTESIAN_POINT ( 'NONE',  ( 0.2000180313179936165, 189.6977690162252657, 10.38967773564543684 ) ) ;
#6377 = LINE ( 'NONE', #13516, #14089 ) ;
#6378 = CARTESIAN_POINT ( 'NONE',  ( -5.783239563508395520, -1.602707436861224632, 12.47358595436692319 ) ) ;
#6379 = CARTESIAN_POINT ( 'NONE',  ( 0.000000000000000000, 2.000000000000000000, -7.000000000000000000 ) ) ;
#6380 = EDGE_LOOP ( 'NONE', ( #3441, #10748, #2372, #10459 ) ) ;
#6381 = CARTESIAN_POINT ( 'NONE',  ( -2.066987300000000083, 187.2499999989075263, 7.000000000000000000 ) ) ;
#6382 = ORIENTED_EDGE ( 'NONE', *, *, #7543, .T. ) ;
#6383 = FACE_OUTER_BOUND ( 'NONE', #14422, .T. ) ;
#6384 = ORIENTED_EDGE ( 'NONE', *, *, #7368, .F. ) ;
#6385 = CARTESIAN_POINT ( 'NONE',  ( -5.666074146197935590, -1.978051345703340180, 25.50004932073311892 ) ) ;
#6386 = DIRECTION ( 'NONE',  ( 0.000000000000000000, 0.000000000000000000, 1.000000000000000000 ) ) ;
#6387 = ORIENTED_EDGE ( 'NONE', *, *, #78, .F. ) ;
#6388 = B_SPLINE_CURVE_WITH_KNOTS ( 'NONE', 3,
 ( #14638, #14716, #5888, #12001, #69, #7164, #1024, #1106, #3647, #10813, #9865, #5969, #6212, #2541, #14473, #2294, #1337, #11048 ),
 .UNSPECIFIED., .F., .F.,
 ( 4, 2, 2, 2, 2, 2, 2, 2, 4 ),
 ( 0.000000000000000000, 0.0003914362731607616401, 0.0007828725463215232801, 0.001174308819482284974, 0.001565745092643046560, 0.001957181365803808363, 0.002348617638964569949, 0.002740053912125331535, 0.003131490185286093120 ),
 .UNSPECIFIED. ) ;
#6389 = CARTESIAN_POINT ( 'NONE',  ( -2.066987299999999639, 0.000000000000000000, 0.4500000010924747329 ) ) ;
#6390 = CARTESIAN_POINT ( 'NONE',  ( 0.9999196734182647095, 5.916093360767514575, 4.867259559550685566 ) ) ;
#6391 = CARTESIAN_POINT ( 'NONE',  ( -2.866007985673219682, 189.8358165770212054, 8.236538289369191190 ) ) ;
#6392 = CARTESIAN_POINT ( 'NONE',  ( -2.066760391300492827E-16, 189.4499999989075150, 4.933012699999999029 ) ) ;
#6393 = CARTESIAN_POINT ( 'NONE',  ( 1.767766952966369320, -1.767766952966368654, 1.199999999999999956 ) ) ;
#6394 = ADVANCED_FACE ( 'NONE', ( #13640, #5313, #2756, #7607, #15482, #5619, #15399, #7997, #11802, #9275, #2174, #5697, #4495, #15558, #5774, #12759, #14037, #667, #6894, #906, #11570, #9349, #12920, #15320, #15239, #3145 ), #10541, .T. ) ;
#6395 = CARTESIAN_POINT ( 'NONE',  ( 0.000000000000000000, 189.6977690162252657, 10.38967773564543862 ) ) ;
#6396 = CONTEXT_DEPENDENT_SHAPE_REPRESENTATION ( #501, #7050 ) ;
#6397 = DIRECTION ( 'NONE',  ( 0.000000000000000000, 0.000000000000000000, -1.000000000000000000 ) ) ;
#6398 = CARTESIAN_POINT ( 'NONE',  ( 2.066987299999999639, 0.8561741729129456191, -0.4999999989075253337 ) ) ;
#6399 = EDGE_CURVE ( 'NONE', #14733, #15393, #2020, .T. ) ;
#6400 = DIRECTION ( 'NONE',  ( -0.9510565162951544194, 0.3090169943749447312, 0.000000000000000000 ) ) ;
#6401 = CARTESIAN_POINT ( 'NONE',  ( -0.1323736289504332531, 6.250000000000000888, 32.00000000000000000 ) ) ;
#6402 = VERTEX_POINT ( 'NONE', #6816 ) ;
#6403 = ORIENTED_EDGE ( 'NONE', *, *, #2065, .T. ) ;
#6404 = ORIENTED_EDGE ( 'NONE', *, *, #6211, .F. ) ;
#6405 = CARTESIAN_POINT ( 'NONE',  ( 0.6156307853270768238, 5.969051238897241873, 18.79870573410680379 ) ) ;
#6406 = CARTESIAN_POINT ( 'NONE',  ( 2.491866687051035978, 189.0000000000000000, 7.260727728595771424 ) ) ;
#6407 = ORIENTED_EDGE ( 'NONE', *, *, #2149, .F. ) ;
#6408 = CARTESIAN_POINT ( 'NONE',  ( 0.7995524673975749064, 6.199337389817269006, 5.614536794524586760 ) ) ;
#6409 = CARTESIAN_POINT ( 'NONE',  ( 2.500000000000000000, 3.061616997868383141E-16, -0.9999999978150501123 ) ) ;
#6410 = EDGE_CURVE ( 'NONE', #12097, #4790, #1864, .T. ) ;
#6411 = CARTESIAN_POINT ( 'NONE',  ( -5.131373506000731055, 7.062729720844018289, 31.00000000000000000 ) ) ;
#6412 = CARTESIAN_POINT ( 'NONE',  ( 5.558508435838239059, -2.857531096718835872, 30.86765874365832119 ) ) ;
#6413 = CARTESIAN_POINT ( 'NONE',  ( 4.743384504624081899E-17, 185.6999999978150697, 4.500000000000000000 ) ) ;
#6414 = LINE ( 'NONE', #10428, #12176 ) ;
#6415 = CARTESIAN_POINT ( 'NONE',  ( 5.531796221294904115, -2.326749136277146857, 12.37378430870260537 ) ) ;
#6416 = CARTESIAN_POINT ( 'NONE',  ( 3.010624175977925532, 5.190832888732251682, 10.70111757752057002 ) ) ;
#6417 = CARTESIAN_POINT ( 'NONE',  ( -9.750000000000003553, 146.0000000000000000, -3.401296724241641415E-14 ) ) ;
#6418 = CARTESIAN_POINT ( 'NONE',  ( -2.500000000000000444, 185.9699999975965454, 7.000000000000000000 ) ) ;
#6419 = CARTESIAN_POINT ( 'NONE',  ( -1.051851325171203388, 227.7069327454752283, 5.392995910236884960 ) ) ;
#6420 = CARTESIAN_POINT ( 'NONE',  ( -1.707413668510289861, 226.4963546398602148, 4.991255295473766118 ) ) ;
#6421 = CARTESIAN_POINT ( 'NONE',  ( -2.347932364728245513, 189.7818114793913367, 9.238878617153785555 ) ) ;
#6422 =( BOUNDED_CURVE ( )  B_SPLINE_CURVE ( 2, ( #10417, #15267, #12865, #1969, #6847, #782, #5645, #3325, #15349 ),
 .UNSPECIFIED., .F., .F. ) 
 B_SPLINE_CURVE_WITH_KNOTS ( ( 3, 2, 2, 2, 3 ),
 ( 0.07142857142857142461, 0.08928571428571428770, 0.1071428571428571369, 0.1250000000000000000, 0.1428571428571428492 ),
 .UNSPECIFIED. ) 
 CURVE ( )  GEOMETRIC_REPRESENTATION_ITEM ( )  RATIONAL_B_SPLINE_CURVE ( ( 1.000000000000000000, 0.9238795325112867385, 1.000000000000000000, 0.9238795325112867385, 1.000000000000000000, 0.9238795325112867385, 1.000000000000000000, 0.9238795325112867385, 1.000000000000000000 ) ) 
 REPRESENTATION_ITEM ( '' )  );
#6423 = ORIENTED_EDGE ( 'NONE', *, *, #2829, .F. ) ;
#6424 = CARTESIAN_POINT ( 'NONE',  ( -7.799024015210657801, -1.482594289697236389, 31.00000000000000000 ) ) ;
#6425 = B_SPLINE_CURVE_WITH_KNOTS ( 'NONE', 3,
 ( #9687, #13562, #12529, #1783, #8730, #6347, #11182, #14847, #9999, #281, #1629, #2833, #5067, #7838, #9048, #11103, #13799, #8808 ),
 .UNSPECIFIED., .F., .F.,
 ( 4, 2, 2, 2, 2, 2, 2, 2, 4 ),
 ( 0.003131918686235977793, 0.003523310662250268063, 0.003914702638264558332, 0.004306094614278849035, 0.004697486590293138004, 0.005088878566307427839, 0.005480270542321717675, 0.005871662518336007511, 0.006263054494350296479 ),
 .UNSPECIFIED. ) ;
#6426 = CYLINDRICAL_SURFACE ( 'NONE', #13713, 1.000000000000000666 ) ;
#6427 = CARTESIAN_POINT ( 'NONE',  ( -13.50000000000000000, 0.000000000000000000, -1.999999999999997113 ) ) ;
#6428 = CARTESIAN_POINT ( 'NONE',  ( 0.7995298244856630099, 5.947211616899221731, 25.11456014619858124 ) ) ;
#6429 = VECTOR ( 'NONE', #631, 1000.000000000000114 ) ;
#6430 = CARTESIAN_POINT ( 'NONE',  ( 2.868718875460478657, 227.0003171668635389, 6.475958485551715604 ) ) ;
#6431 = B_SPLINE_CURVE_WITH_KNOTS ( 'NONE', 3,
 ( #3921, #3845, #13627, #2505, #2820, #14599, #14912, #5053, #4979, #12517, #3690, #4003, #270, #8881, #11170, #6094, #5133, #14835 ),
 .UNSPECIFIED., .F., .F.,
 ( 4, 2, 2, 2, 2, 2, 2, 2, 4 ),
 ( 0.003131486019302005472, 0.003522824630466710009, 0.003914163241631414547, 0.004305501852796118217, 0.004696840463960822755, 0.005088179075125527293, 0.005479517686290230963, 0.005870856297454935500, 0.006262194908619640038 ),
 .UNSPECIFIED. ) ;
#6432 = FACE_OUTER_BOUND ( 'NONE', #4078, .T. ) ;
#6433 = CARTESIAN_POINT ( 'NONE',  ( 4.592425496802573972E-16, -2.500000000000000000, 1.100000000000000089 ) ) ;
#6434 = CARTESIAN_POINT ( 'NONE',  ( -4.154121946521065922, 4.670585111242799847, 23.70112161576661336 ) ) ;
#6435 = EDGE_CURVE ( 'NONE', #9302, #13528, #3169, .T. ) ;
#6436 = DIRECTION ( 'NONE',  ( 0.000000000000000000, 0.000000000000000000, 1.000000000000000000 ) ) ;
#6437 = CARTESIAN_POINT ( 'NONE',  ( -6.437450399132682577E-16, 187.0000000000000000, 9.500000000000001776 ) ) ;
#6438 = CARTESIAN_POINT ( 'NONE',  ( 1.767766952966369320, -1.767766952966368654, -1.899999997815050357 ) ) ;
#6439 = CARTESIAN_POINT ( 'NONE',  ( 1.214181464861975757, 227.7437454098885041, 5.499312984720448938 ) ) ;
#6440 = CARTESIAN_POINT ( 'NONE',  ( -2.066987299999999639, 0.8561741729129455081, -2.599999998907525089 ) ) ;
#6441 = CARTESIAN_POINT ( 'NONE',  ( -1.767766952966369098, 1.767766952966369098, -3.099999997815050090 ) ) ;
#6442 = DIRECTION ( 'NONE',  ( 0.000000000000000000, 0.000000000000000000, 1.000000000000000000 ) ) ;
#6443 = CARTESIAN_POINT ( 'NONE',  ( -2.500000000000000444, 184.3499999999999943, 5.964466094067261359 ) ) ;
#6444 = CARTESIAN_POINT ( 'NONE',  ( -3.107688324358827803, 5.133887830459763713, 18.87378430870261781 ) ) ;
#6446 = VERTEX_POINT ( 'NONE', #8159 ) ;
#6445 = CARTESIAN_POINT ( 'NONE',  ( 1.461580736456472795, 187.7499999989075263, 5.538419263543527649 ) ) ;
#6447 = FACE_OUTER_BOUND ( 'NONE', #3585, .T. ) ;
#6448 = CARTESIAN_POINT ( 'NONE',  ( -1.767766952966369765, 186.7999999978150356, 8.767766952966368876 ) ) ;
#6449 = CIRCLE ( 'NONE', #5678, 1.499999999999999556 ) ;
#6450 = CARTESIAN_POINT ( 'NONE',  ( 0.09128442572522987852, 0.4000000000000062395, -2.551849451881606168 ) ) ;
#6451 = SURFACE_SIDE_STYLE ('',( #1728 ) ) ;
#6452 = CARTESIAN_POINT ( 'NONE',  ( 5.665824935993679645, -1.978765057080718481, 25.49995053646222232 ) ) ;
#6453 = EDGE_CURVE ( 'NONE', #4873, #10357, #11727, .T. ) ;
#6454 = CARTESIAN_POINT ( 'NONE',  ( 1.724409861001041877, 189.4160653832104231, 4.535432872984458186 ) ) ;
#6455 = CARTESIAN_POINT ( 'NONE',  ( 0.07473532696167239919, -0.3999999999999941380, -2.548950835425553674 ) ) ;
#6456 = CARTESIAN_POINT ( 'NONE',  ( 1.049294306888729489, 190.0690657775611214, 4.388349470883383674 ) ) ;
#6457 = DIRECTION ( 'NONE',  ( -0.5877852522924685852, -0.8090169943749507819, 0.000000000000000000 ) ) ;
#6458 = DIRECTION ( 'NONE',  ( -0.000000000000000000, -1.000000000000000000, -0.000000000000000000 ) ) ;
#6459 = CARTESIAN_POINT ( 'NONE',  ( 4.286401442266388528, 4.198423832313340043, 24.49999999999999289 ) ) ;
#6460 = VERTEX_POINT ( 'NONE', #3066 ) ;
#6461 = CARTESIAN_POINT ( 'NONE',  ( -0.8561741729129469514, 187.3999999989075889, 9.066987299999999195 ) ) ;
#6462 = VECTOR ( 'NONE', #4428, 1000.000000000000114 ) ;
#6463 = ORIENTED_EDGE ( 'NONE', *, *, #9693, .T. ) ;
#6464 = CARTESIAN_POINT ( 'NONE',  ( -5.935543223013818981, -0.8771126767609508379, 24.36763921416088863 ) ) ;
#6465 = VERTEX_POINT ( 'NONE', #2099 ) ;
#6466 = CARTESIAN_POINT ( 'NONE',  ( -5.531623157106079880, -2.327208526676637579, 25.37364704684422634 ) ) ;
#6467 = DIRECTION ( 'NONE',  ( 0.000000000000000000, 1.000000000000000000, 0.000000000000000000 ) ) ;
#6468 = EDGE_LOOP ( 'NONE', ( #11219, #3116 ) ) ;
#6469 = CARTESIAN_POINT ( 'NONE',  ( 2.066987299999999639, 2.531329380823229670E-16, 0.05000000109247476621 ) ) ;
#6470 = CARTESIAN_POINT ( 'NONE',  ( -0.9740807849834816068, 5.920620690450712154, 17.73850119700669126 ) ) ;
#6471 = CARTESIAN_POINT ( 'NONE',  ( -1.409930671981111772, 189.7264147913530223, 10.03734922520923867 ) ) ;
#6472 = CARTESIAN_POINT ( 'NONE',  ( -7.490007020835642848, -2.433650805992559896, 24.49999999999999289 ) ) ;
#6473 = CARTESIAN_POINT ( 'NONE',  ( -1.035533905932738197, -2.500000000000000000, -2.150000000000000355 ) ) ;
#6474 = CARTESIAN_POINT ( 'NONE',  ( 9.750000000000003553, -1.020968533498575335E-13, 2.000000000000001776 ) ) ;
#6475 = CARTESIAN_POINT ( 'NONE',  ( 3.010624175978041883, -5.190832888732185957, 31.79888242247942642 ) ) ;
#6476 = CARTESIAN_POINT ( 'NONE',  ( 2.066987299999999639, 2.531329380823229670E-16, -1.349999998907525534 ) ) ;
#6477 = DIRECTION ( 'NONE',  ( -0.3090169943749584425, 0.9510565162951498674, 0.000000000000000000 ) ) ;
#6478 = CARTESIAN_POINT ( 'NONE',  ( 4.286401442266483564, 4.198423832313243231, 11.63239388001634289 ) ) ;
#6479 = ORIENTED_EDGE ( 'NONE', *, *, #9122, .F. ) ;
#6480 = ORIENTED_EDGE ( 'NONE', *, *, #12636, .F. ) ;
#6481 = ORIENTED_EDGE ( 'NONE', *, *, #7412, .F. ) ;
#6482 = CARTESIAN_POINT ( 'NONE',  ( 5.867109477881242263, -1.259218163100928267, 30.20111757752059489 ) ) ;
#6483 = CARTESIAN_POINT ( 'NONE',  ( -2.500000000000000888, 187.5999999999999943, 7.000000000000000000 ) ) ;
#6484 = EDGE_LOOP ( 'NONE', ( #5849, #14235, #10927, #12810 ) ) ;
#6485 = CARTESIAN_POINT ( 'NONE',  ( 0.9999171162589708395, 6.169494774098548184, 4.867223203306743073 ) ) ;
#6486 = CARTESIAN_POINT ( 'NONE',  ( 6.176542424588140179, -0.9554180641284089059, 17.99999999999998934 ) ) ;
#6487 = AXIS2_PLACEMENT_3D ( 'NONE', #1755, #636, #4225 ) ;
#6488 = DIRECTION ( 'NONE',  ( 1.000000000000000000, 0.000000000000000000, 0.000000000000000000 ) ) ;
#6489 = CARTESIAN_POINT ( 'NONE',  ( 5.985119669071122139, -1.805077827356540432, 30.00008258189710730 ) ) ;
#6490 = CARTESIAN_POINT ( 'NONE',  ( 1.035533905932738197, 186.9499999978150413, 9.500000000000003553 ) ) ;
#6491 = SURFACE_STYLE_USAGE ( .BOTH. , #2739 ) ;
#6492 = CARTESIAN_POINT ( 'NONE',  ( 2.500000000000000000, 3.061616997868383141E-16, 1.306999999978150528 ) ) ;
#6493 = CARTESIAN_POINT ( 'NONE',  ( 0.000000000000000000, 0.000000000000000000, -13.50000000000000000 ) ) ;
#6494 = DIRECTION ( 'NONE',  ( 0.000000000000000000, -1.000000000000000000, 0.000000000000000000 ) ) ;
#6495 = CARTESIAN_POINT ( 'NONE',  ( -2.500000000000000444, 187.5199999975965568, 5.964466094067261359 ) ) ;
#6496 = CARTESIAN_POINT ( 'NONE',  ( -0.2609190394019921810, 228.9066108255455276, 8.857734630635405892 ) ) ;
#6497 = CARTESIAN_POINT ( 'NONE',  ( -2.599095426179941271, 226.8075136295145171, 5.908139701444540925 ) ) ;
#6498 = EDGE_CURVE ( 'NONE', #5516, #11747, #9510, .T. ) ;
#6499 = CARTESIAN_POINT ( 'NONE',  ( -2.568556045599829751, 189.1887412497518142, 8.730119828325975107 ) ) ;
#6500 = B_SPLINE_CURVE_WITH_KNOTS ( 'NONE', 3,
 ( #2053, #10498, #13030, #13108, #5574, #8195, #12791, #14065, #5496, #9463, #4449, #12952, #12869, #10340, #10571, #3099, #8271, #11602 ),
 .UNSPECIFIED., .F., .F.,
 ( 4, 2, 2, 2, 2, 2, 2, 2, 4 ),
 ( 0.000000000000000000, 0.0003914904498596246296, 0.0007829808997192490424, 0.001174471349578873293, 0.001565961799438497868, 0.001957452249298122227, 0.002348942699157746585, 0.002740433149017371811, 0.003131923598876996170 ),
 .UNSPECIFIED. ) ;
#6501 = ORIENTED_EDGE ( 'NONE', *, *, #939, .T. ) ;
#6502 = EDGE_CURVE ( 'NONE', #14180, #6446, #6165, .T. ) ;
#6503 = CARTESIAN_POINT ( 'NONE',  ( -2.849269941561985764, 5.281123252784034605, 5.615193824488510010 ) ) ;
#6504 = DIRECTION ( 'NONE',  ( 0.000000000000000000, 0.000000000000000000, 1.000000000000000000 ) ) ;
#6505 = CARTESIAN_POINT ( 'NONE',  ( 0.8736772044960799954, -6.188841968496048729, 10.99611573292812672 ) ) ;
#6506 = DIRECTION ( 'NONE',  ( 0.000000000000000000, 0.000000000000000000, 1.000000000000000000 ) ) ;
#6507 = CARTESIAN_POINT ( 'NONE',  ( 2.777531521503771472, 227.6543197073591216, 8.401223264750537822 ) ) ;
#6508 = CARTESIAN_POINT ( 'NONE',  ( 3.568242062701532546, 5.132954954975506467, 6.000049068765333615 ) ) ;
#6509 = CARTESIAN_POINT ( 'NONE',  ( -2.066987299999999195, -0.8561741729129466183, -2.499999998907525001 ) ) ;
#6510 = CARTESIAN_POINT ( 'NONE',  ( 3.419318284370227445, 4.932111238568157141, 4.000079976437387330 ) ) ;
#6511 = CIRCLE ( 'NONE', #2152, 2.649388036945190095 ) ;
#6512 = CARTESIAN_POINT ( 'NONE',  ( -1.524659305057740610E-16, 189.0000000000000000, 4.500000000000000000 ) ) ;
#6513 = CARTESIAN_POINT ( 'NONE',  ( 1.035533905932738197, 186.2500000000000000, 9.500000000000003553 ) ) ;
#6514 =( REPRESENTATION_RELATIONSHIP ('NONE','NONE', #11191, #4596 ) REPRESENTATION_RELATIONSHIP_WITH_TRANSFORMATION ( #7110 )SHAPE_REPRESENTATION_RELATIONSHIP( ) );
#6515 = CARTESIAN_POINT ( 'NONE',  ( 0.2606415164794526063, 227.6142277459897230, 5.125258584176975774 ) ) ;
#6516 = CARTESIAN_POINT ( 'NONE',  ( -3.000000000000000444, -1.732050807568878081, -5.500000000000000000 ) ) ;
#6517 = CARTESIAN_POINT ( 'NONE',  ( -4.435347140101057128, -4.403429997944488861, 11.36936067245786219 ) ) ;
#6518 = DIRECTION ( 'NONE',  ( 1.000000000000000000, 0.000000000000000000, 0.000000000000000000 ) ) ;
#6519 = CARTESIAN_POINT ( 'NONE',  ( -2.500000000000000444, 184.4000000000000057, 7.000000000000000000 ) ) ;
#6520 = CARTESIAN_POINT ( 'NONE',  ( 6.081590040723110491, -1.446205118472867923, 18.87367328635991726 ) ) ;
#6522 = VERTEX_POINT ( 'NONE', #14263 ) ;
#6521 = CARTESIAN_POINT ( 'NONE',  ( 2.066987299999999639, 189.2999999989075661, 6.143825827087054492 ) ) ;
#6523 = DIRECTION ( 'NONE',  ( -0.3090169943749584425, 0.9510565162951498674, 0.000000000000000000 ) ) ;
#6524 = CARTESIAN_POINT ( 'NONE',  ( 6.172651332693103399, -0.9815532474593076095, 11.76190213084010239 ) ) ;
#6525 = CARTESIAN_POINT ( 'NONE',  ( -5.915653884842720700, 1.003805156977363833, 4.495602393557862619 ) ) ;
#6526 = CARTESIAN_POINT ( 'NONE',  ( 2.136295798034152149, 189.1395851565150679, 9.290070378363166625 ) ) ;
#6527 = LINE ( 'NONE', #11362, #4278 ) ;
#6528 = AXIS2_PLACEMENT_3D ( 'NONE', #13498, #4111, #2921 ) ;
#6529 = CARTESIAN_POINT ( 'NONE',  ( 3.106366801612069573, -5.134708448381242185, 5.873037790270517533 ) ) ;
#6530 = CARTESIAN_POINT ( 'NONE',  ( 6.081836621194488757, -1.445163676684627641, 23.62694108445698760 ) ) ;
#6531 = CYLINDRICAL_SURFACE ( 'NONE', #918, 3.000000000000000888 ) ;
#6532 = CARTESIAN_POINT ( 'NONE',  ( -5.531209434046302498, -2.328189801702702511, 10.62696220972947003 ) ) ;
#6533 = EDGE_LOOP ( 'NONE', ( #12075, #1428 ) ) ;
#6534 = CARTESIAN_POINT ( 'NONE',  ( -0.8561741729129456191, 187.8999999989075320, 4.933012699999999029 ) ) ;
#6535 = ORIENTED_EDGE ( 'NONE', *, *, #8176, .F. ) ;
#6536 = DIRECTION ( 'NONE',  ( -0.9510565162951545304, 0.3090169943749447867, 0.000000000000000000 ) ) ;
#6537 = ORIENTED_EDGE ( 'NONE', *, *, #8094, .T. ) ;
#6538 = EDGE_CURVE ( 'NONE', #10984, #8231, #10750, .T. ) ;
#6539 = FACE_OUTER_BOUND ( 'NONE', #13454, .T. ) ;
#6540 = PRESENTATION_STYLE_ASSIGNMENT (( #6620 ) ) ;
#6541 = B_SPLINE_CURVE_WITH_KNOTS ( 'NONE', 3,
 ( #12508, #12431, #1606, #9900, #1374, #2496, #12195, #11317, #340, #416, #106, #4077, #8948, #2731, #12352, #1531, #7355, #6406, #11163, #11238, #6247, #4973, #14753, #9824, #3761, #1446, #5124, #9977, #14828, #3913, #8789, #13619 ),
 .UNSPECIFIED., .F., .F.,
 ( 4, 2, 2, 2, 2, 2, 2, 2, 2, 2, 2, 2, 2, 2, 2, 4 ),
 ( 0.2688658829390630500, 0.3001158843412741750, 0.3313658857434852445, 0.3626158871456963695, 0.3938658885479074945, 0.4251158899501185640, 0.4563658913523296889, 0.4876158927545407584, 0.5188658941567521055, 0.5501158955589633415, 0.5813658969611745775, 0.6126158983633858135, 0.6438658997655970495, 0.7063659025700197436, 0.7376159039722309796, 0.7688659053744424376 ),
 .UNSPECIFIED. ) ;
#6542 = CIRCLE ( 'NONE', #15422, 1.499999999999999556 ) ;
#6543 = ORIENTED_EDGE ( 'NONE', *, *, #4975, .T. ) ;
#6544 = CARTESIAN_POINT ( 'NONE',  ( -2.066987299999999195, -0.8561741729129466183, -1.099999998907525089 ) ) ;
#6545 = CARTESIAN_POINT ( 'NONE',  ( -0.9999502950800709389, 5.916088184763905744, 18.13108149190012597 ) ) ;
#6546 = CARTESIAN_POINT ( 'NONE',  ( 7.000000000000006217, 0.000000000000000000, 0.000000000000000000 ) ) ;
#6547 = CARTESIAN_POINT ( 'NONE',  ( -1.767766952966368432, -1.767766952966369320, -2.200000000000000178 ) ) ;
#6548 = CARTESIAN_POINT ( 'NONE',  ( -1.035533905932738197, -2.500000000000000000, -1.350000000000000089 ) ) ;
#6549 = CARTESIAN_POINT ( 'NONE',  ( 0.000000000000000000, 2.000000000000000000, 0.000000000000000000 ) ) ;
#6550 = LINE ( 'NONE', #11309, #12064 ) ;
#6551 = CARTESIAN_POINT ( 'NONE',  ( 1.461580736456472573, 1.461580736456472795, 1.150000001092474911 ) ) ;
#6552 = CARTESIAN_POINT ( 'NONE',  ( -0.9740856415300650495, 6.173834621338596840, 30.73852653055532613 ) ) ;
#6553 = EDGE_LOOP ( 'NONE', ( #12113, #11059 ) ) ;
#6554 = ORIENTED_EDGE ( 'NONE', *, *, #8097, .T. ) ;
#6555 = VERTEX_POINT ( 'NONE', #3535 ) ;
#6556 = CARTESIAN_POINT ( 'NONE',  ( -5.903061651806586596, -2.057626436184838870, 10.50008258189709132 ) ) ;
#6557 = FACE_OUTER_BOUND ( 'NONE', #7948, .T. ) ;
#6558 = ORIENTED_EDGE ( 'NONE', *, *, #9926, .F. ) ;
#6559 = AXIS2_PLACEMENT_3D ( 'NONE', #8410, #13245, #2343 ) ;
#6560 = ADVANCED_FACE ( 'NONE', ( #2336, #2419, #12201, #8318, #13157, #9755 ), #6252, .T. ) ;
#6561 = CARTESIAN_POINT ( 'NONE',  ( -5.558508435838126260, -2.857531096719055252, 17.99999999999998934 ) ) ;
#6562 = CARTESIAN_POINT ( 'NONE',  ( 0.6139731865241387920, -6.220476368274037604, 17.19975545601932865 ) ) ;
#6563 = CIRCLE ( 'NONE', #10601, 1.499999999999999556 ) ;
#6564 = CARTESIAN_POINT ( 'NONE',  ( -0.9735954530124010242, 6.173909381474013358, 18.26281793585238233 ) ) ;
#6565 = CARTESIAN_POINT ( 'NONE',  ( 0.7995524673976397434, 6.199337389817260124, 18.61453679452466403 ) ) ;
#6566 = CARTESIAN_POINT ( 'NONE',  ( 1.767766952966368654, 185.3999999978150584, 8.767766952966368876 ) ) ;
#6567 = CARTESIAN_POINT ( 'NONE',  ( 1.767766952966369320, 184.7999999978150356, 5.232233047033630235 ) ) ;
#6568 = CARTESIAN_POINT ( 'NONE',  ( 3.633127580202213380, 4.776802569231102247, 10.49992038825521590 ) ) ;
#6569 = CARTESIAN_POINT ( 'NONE',  ( 9.750000000000003553, 186.0000000000000000, 1.020968533498575461E-13 ) ) ;
#6570 = CARTESIAN_POINT ( 'NONE',  ( -1.035533905932737975, 187.4199999975965909, 4.500000000000000888 ) ) ;
#6571 = CARTESIAN_POINT ( 'NONE',  ( 1.455795469679321608, 228.1339131991090596, 9.811868761735363265 ) ) ;
#6572 = CARTESIAN_POINT ( 'NONE',  ( -2.951760543192366804, 227.4626507460308744, 7.837199003427246069 ) ) ;
#6573 = AXIS2_PLACEMENT_3D ( 'NONE', #8767, #13676, #7794 ) ;
#6574 = VERTEX_POINT ( 'NONE', #12123 ) ;
#6575 = CARTESIAN_POINT ( 'NONE',  ( -1.767766952966368432, -1.767766952966369320, 0.3000000021849498211 ) ) ;
#6576 = ORIENTED_EDGE ( 'NONE', *, *, #3749, .F. ) ;
#6577 = CARTESIAN_POINT ( 'NONE',  ( -3.107688324358700349, 5.133887830459841872, 5.873784308702619583 ) ) ;
#6578 = CARTESIAN_POINT ( 'NONE',  ( 2.996417732210587381, -5.485687819086892958, 10.88603820591927196 ) ) ;
#6579 = CARTESIAN_POINT ( 'NONE',  ( -0.5039005892421214439, 6.230833003620541710, 4.126363889112979244 ) ) ;
#6580 = CARTESIAN_POINT ( 'NONE',  ( 5.570760634536775058, 2.834026536768299298, 30.73774718278284013 ) ) ;
#6581 = CYLINDRICAL_SURFACE ( 'NONE', #2583, 1.000000000000000444 ) ;
#6582 = AXIS2_PLACEMENT_3D ( 'NONE', #10946, #11891, #3464 ) ;
#6583 = CARTESIAN_POINT ( 'NONE',  ( -5.317509234263930296, -2.779225709351048401, 5.000000000000004441 ) ) ;
#6584 = CARTESIAN_POINT ( 'NONE',  ( 1.461580736456473018, -1.461580736456472573, -2.249999998907525445 ) ) ;
#6585 = DIRECTION ( 'NONE',  ( -1.062480551894329468E-17, -3.608224830031754812E-16, 1.000000000000000000 ) ) ;
#6586 = CARTESIAN_POINT ( 'NONE',  ( -3.567624405365240836, -5.133384272590781450, 30.00004921015706572 ) ) ;
#6587 = CARTESIAN_POINT ( 'NONE',  ( 1.035533905932738419, 184.6500000000000057, 9.500000000000003553 ) ) ;
#6588 = ADVANCED_FACE ( 'NONE', ( #7206 ), #4819, .T. ) ;
#6589 = CARTESIAN_POINT ( 'NONE',  ( 0.9680444063220374762, 227.6910878243089087, 5.347234874174658259 ) ) ;
#6590 = PRODUCT_DEFINITION_CONTEXT ( 'detailed design', #12674, 'design' ) ;
#6591 = FACE_BOUND ( 'NONE', #7894, .T. ) ;
#6592 = CARTESIAN_POINT ( 'NONE',  ( -1.035533905932738197, -2.500000000000000000, -2.849999997815050978 ) ) ;
#6593 = CARTESIAN_POINT ( 'NONE',  ( -1.461580736456472795, 1.461580736456472795, -1.249999998907525223 ) ) ;
#6594 = CARTESIAN_POINT ( 'NONE',  ( 9.147955830346443662E-17, 185.0000000000000000, 4.500000000000000000 ) ) ;
#6595 = CARTESIAN_POINT ( 'NONE',  ( 5.770331821586463406, -2.404225004693450352, 18.87380055247394850 ) ) ;
#6597 = ORIENTED_EDGE ( 'NONE', *, *, #9514, .F. ) ;
#6596 = CARTESIAN_POINT ( 'NONE',  ( -1.461580736456473018, 187.9499999989075150, 5.538419263543527649 ) ) ;
#6598 = CARTESIAN_POINT ( 'NONE',  ( -2.849269941562030173, -5.281123252784012401, 17.38480617551148200 ) ) ;
#6599 = ADVANCED_FACE ( 'NONE', ( #10936 ), #2504, .F. ) ;
#6600 = CARTESIAN_POINT ( 'NONE',  ( 2.500000000000000444, 187.0999999978150754, 7.000000000000000000 ) ) ;
#6601 = CARTESIAN_POINT ( 'NONE',  ( -5.999999999999999112, 186.5669965222008670, 9.317226423031115701 ) ) ;
#6602 = EDGE_CURVE ( 'NONE', #1820, #14280, #13231, .T. ) ;
#6603 = DIRECTION ( 'NONE',  ( -0.000000000000000000, 1.000000000000000000, -0.000000000000000000 ) ) ;
#6604 = CARTESIAN_POINT ( 'NONE',  ( 2.975469271411296024, 189.2669713358625643, 7.607624869344640217 ) ) ;
#6605 = AXIS2_PLACEMENT_3D ( 'NONE', #5887, #10734, #2211 ) ;
#6606 = DIRECTION ( 'NONE',  ( 0.8090169943749421222, 0.5877852522924802425, 0.000000000000000000 ) ) ;
#6607 = CARTESIAN_POINT ( 'NONE',  ( -0.2622916576876348493, 5.995491482261827265, 31.97384942646813855 ) ) ;
#6608 = CARTESIAN_POINT ( 'NONE',  ( 3.311576095066638636, -5.004818610361268405, 5.973778239432936843 ) ) ;
#6609 = CARTESIAN_POINT ( 'NONE',  ( 6.081590040723080293, -1.446205118472996931, 5.873673286359928802 ) ) ;
#6610 = CARTESIAN_POINT ( 'NONE',  ( 2.094888807778566729E-14, 6.000000000000000888, 30.00000000000000000 ) ) ;
#6611 = CARTESIAN_POINT ( 'NONE',  ( -7.490007020835664164, -2.433650805992495503, 17.99999999999998934 ) ) ;
#6612 = EDGE_CURVE ( 'NONE', #6278, #4624, #3450, .T. ) ;
#6613 = ORIENTED_EDGE ( 'NONE', *, *, #14246, .F. ) ;
#6614 = CARTESIAN_POINT ( 'NONE',  ( 2.066987299999999639, 186.7999999989074809, 7.856174172912946396 ) ) ;
#6615 = VERTEX_POINT ( 'NONE', #9587 ) ;
#6616 = DIRECTION ( 'NONE',  ( -0.5877852522924685852, -0.8090169943749507819, 0.000000000000000000 ) ) ;
#6617 =( GEOMETRIC_REPRESENTATION_CONTEXT ( 3 ) GLOBAL_UNCERTAINTY_ASSIGNED_CONTEXT ( ( #12617 ) ) GLOBAL_UNIT_ASSIGNED_CONTEXT ( ( #9056, #2915, #7766 ) ) REPRESENTATION_CONTEXT ( 'NONE', 'WORKASPACE' ) );
#6618 = ORIENTED_EDGE ( 'NONE', *, *, #14471, .F. ) ;
#6619 = FACE_OUTER_BOUND ( 'NONE', #6687, .T. ) ;
#6620 = SURFACE_STYLE_USAGE ( .BOTH. , #4295 ) ;
#6621 = ORIENTED_EDGE ( 'NONE', *, *, #14856, .T. ) ;
#6622 = CARTESIAN_POINT ( 'NONE',  ( 1.461580736456473018, -1.461580736456472573, -2.449999998907525622 ) ) ;
#6623 = CARTESIAN_POINT ( 'NONE',  ( -4.435347140101074004, 4.403429997944469321, 5.000000000000004441 ) ) ;
#6624 = FACE_OUTER_BOUND ( 'NONE', #1372, .T. ) ;
#6625 = CARTESIAN_POINT ( 'NONE',  ( -1.035533905932737753, 2.500000000000000444, -2.450000000000000178 ) ) ;
#6626 = CARTESIAN_POINT ( 'NONE',  ( 2.500000000000000444, 1.035533905932737975, 2.149999999999999911 ) ) ;
#6627 = CARTESIAN_POINT ( 'NONE',  ( -3.420659742068348219, -4.931142898501759575, 10.50004946353775637 ) ) ;
#6628 = CONTEXT_DEPENDENT_SHAPE_REPRESENTATION ( #8128, #12868 ) ;
#6629 = CARTESIAN_POINT ( 'NONE',  ( 7.490007020835748541, -2.433650805992050969, 24.49999999999999289 ) ) ;
#6630 = CARTESIAN_POINT ( 'NONE',  ( -2.066987299999999195, -0.8561741729129466183, -1.699999998907525400 ) ) ;
#6631 = EDGE_CURVE ( 'NONE', #13293, #2588, #9829, .T. ) ;
#6632 = AXIS2_PLACEMENT_3D ( 'NONE', #2037, #11670, #10484 ) ;
#6633 = CARTESIAN_POINT ( 'NONE',  ( 0.000000000000000000, 19.99999999999999645, 0.000000000000000000 ) ) ;
#6634 = ORIENTED_EDGE ( 'NONE', *, *, #13896, .F. ) ;
#6635 = PRODUCT_RELATED_PRODUCT_CATEGORY ( 'part', '', ( #6900 ) ) ;
#6636 = VERTEX_POINT ( 'NONE', #14678 ) ;
#6637 = VERTEX_POINT ( 'NONE', #3767 ) ;
#6638 = CARTESIAN_POINT ( 'NONE',  ( 3.253823204785158296, -5.337590213880479162, 12.37305891554298931 ) ) ;
#6639 = CARTESIAN_POINT ( 'NONE',  ( 5.770331821586379029, 2.404225004693657297, 4.126199447526043507 ) ) ;
#6640 = VERTEX_POINT ( 'NONE', #8645 ) ;
#6641 = CARTESIAN_POINT ( 'NONE',  ( 2.500000000000000444, 1.035533905932737975, 1.450000002184949732 ) ) ;
#6642 = CARTESIAN_POINT ( 'NONE',  ( -3.458467055437286053, 5.207305717053834826, 31.97359571723301741 ) ) ;
#6643 = CARTESIAN_POINT ( 'NONE',  ( -1.035533905932738197, -2.500000000000000000, -2.150000000000000355 ) ) ;
#6644 = CARTESIAN_POINT ( 'NONE',  ( 1.035533905932737753, 187.2499999978151095, 4.500000000000000888 ) ) ;
#6645 = CARTESIAN_POINT ( 'NONE',  ( -1.767766952966369098, 184.9999999978150527, 5.232233047033630235 ) ) ;
#6646 = DIRECTION ( 'NONE',  ( 1.062480551894331009E-17, -2.775557561562888393E-16, 1.000000000000000000 ) ) ;
#6647 = DIRECTION ( 'NONE',  ( 0.000000000000000000, -1.000000000000000000, 0.000000000000000000 ) ) ;
#6648 = CARTESIAN_POINT ( 'NONE',  ( -2.500000000000000888, 188.3699999975965511, 7.000000000000000000 ) ) ;
#6649 = CARTESIAN_POINT ( 'NONE',  ( -1.580502612156455822, 228.6570661798589299, 8.137035460797768849 ) ) ;
#6650 = CARTESIAN_POINT ( 'NONE',  ( -2.692660167145737304, 226.8630334657495666, 6.071693271619351684 ) ) ;
#6651 = ADVANCED_FACE ( 'NONE', ( #13475 ), #10778, .T. ) ;
#6652 = AXIS2_PLACEMENT_3D ( 'NONE', #848, #14051, #3160 ) ;
#6653 = EDGE_LOOP ( 'NONE', ( #12986, #11392 ) ) ;
#6654 = CARTESIAN_POINT ( 'NONE',  ( 3.312524433819890035, -5.004191858253928871, 4.025919472168997260 ) ) ;
#6655 = ORIENTED_EDGE ( 'NONE', *, *, #3461, .T. ) ;
#6656 = CARTESIAN_POINT ( 'NONE',  ( -3.781065399486098322, 4.978303713186375212, 17.00008258189709309 ) ) ;
#6657 = DIRECTION ( 'NONE',  ( -0.3090169943749447867, -0.9510565162951544194, 0.000000000000000000 ) ) ;
#6658 = CARTESIAN_POINT ( 'NONE',  ( -0.8561741729129456191, 184.4999999989074979, 4.933012699999999029 ) ) ;
#6659 = DIRECTION ( 'NONE',  ( -0.000000000000000000, -1.000000000000000000, -0.000000000000000000 ) ) ;
#6660 = CARTESIAN_POINT ( 'NONE',  ( 2.763116275831466240, 226.9137948392856572, 6.221213813064390585 ) ) ;
#6661 = CARTESIAN_POINT ( 'NONE',  ( 4.290381260516283213, 4.545736887716198105, 5.615177803758427899 ) ) ;
#6662 = CARTESIAN_POINT ( 'NONE',  ( -2.500000000000000000, -1.035533905932739307, 1.750000000000000000 ) ) ;
#6663 = CARTESIAN_POINT ( 'NONE',  ( 1.767766952966369320, -1.767766952966368654, -0.4000000000000001887 ) ) ;
#6664 = CARTESIAN_POINT ( 'NONE',  ( 4.141923667210649640, 4.342011609040460129, 4.384382673013946352 ) ) ;
#6665 =( LENGTH_UNIT ( ) NAMED_UNIT ( * ) SI_UNIT ( .MILLI., .METRE. ) );
#6666 = CARTESIAN_POINT ( 'NONE',  ( -3.458467055437213666, -5.207305717053880123, 30.02640428276698259 ) ) ;
#6667 = CARTESIAN_POINT ( 'NONE',  ( 2.500000000000000444, 186.3499999999999943, 8.035533905932739529 ) ) ;
#6668 = CARTESIAN_POINT ( 'NONE',  ( -1.923034433439944513, 228.0917019039344495, 6.504231185664401949 ) ) ;
#6669 = DIRECTION ( 'NONE',  ( 0.000000000000000000, 0.000000000000000000, -1.000000000000000000 ) ) ;
#6670 = CARTESIAN_POINT ( 'NONE',  ( 6.176542424588121527, -0.9554180641285238140, 31.00000000000000000 ) ) ;
#6671 = CARTESIAN_POINT ( 'NONE',  ( 0.8561741729129465073, -2.066987299999999195, -0.8999999989075251339 ) ) ;
#6672 = CARTESIAN_POINT ( 'NONE',  ( -1.767766952966369320, 186.7000000000000171, 5.232233047033630235 ) ) ;
#6673 = CARTESIAN_POINT ( 'NONE',  ( -2.931156713028654437, 5.520271803279126033, 25.00436969680153965 ) ) ;
#6675 = EDGE_LOOP ( 'NONE', ( #10608, #6145, #2357, #7425 ) ) ;
#6674 = CARTESIAN_POINT ( 'NONE',  ( 0.8561741729129458411, 188.2999999989075093, 9.066987299999999195 ) ) ;
#6676 = EDGE_CURVE ( 'NONE', #12347, #12272, #3859, .T. ) ;
#6677 = CARTESIAN_POINT ( 'NONE',  ( 6.123233995736766282E-16, -6.250000000000000888, 6.000000000000004441 ) ) ;
#6678 = CARTESIAN_POINT ( 'NONE',  ( 4.267936573529090616, 4.217499624512361045, 24.76229037835931734 ) ) ;
#6679 = CARTESIAN_POINT ( 'NONE',  ( -5.329907877631393731, 2.755840666746176559, 4.738056759968538145 ) ) ;
#6680 = CARTESIAN_POINT ( 'NONE',  ( 0.000000000000000000, 0.000000000000000000, 0.000000000000000000 ) ) ;
#6681 = CARTESIAN_POINT ( 'NONE',  ( 2.879399905582539887, 189.9211542764968215, 6.401088131731365927 ) ) ;
#6682 = CARTESIAN_POINT ( 'NONE',  ( -5.317509234263931184, -2.779225709351047957, 5.130649613488544425 ) ) ;
#6683 = CARTESIAN_POINT ( 'NONE',  ( 0.4515139163396761357, 228.8949857255690290, 8.824160678851793449 ) ) ;
#6684 = CARTESIAN_POINT ( 'NONE',  ( -3.736532060718004811, 4.696070028785960027, 30.02622176056705428 ) ) ;
#6685 = CARTESIAN_POINT ( 'NONE',  ( -1.461580736456472795, 1.461580736456472795, 2.150000001092474911 ) ) ;
#6686 = LINE ( 'NONE', #7710, #11021 ) ;
#6687 = EDGE_LOOP ( 'NONE', ( #2494, #14256, #2246, #6987 ) ) ;
#6688 = CARTESIAN_POINT ( 'NONE',  ( -0.8561741729129456191, 188.6999999989075150, 4.933012699999999029 ) ) ;
#6689 = ORIENTED_EDGE ( 'NONE', *, *, #9503, .T. ) ;
#6690 = CARTESIAN_POINT ( 'NONE',  ( 2.668367453516610865, 5.373994336898140212, 31.00000000000000000 ) ) ;
#6691 = ADVANCED_FACE ( 'NONE', ( #2895 ), #10594, .T. ) ;
#6692 = ORIENTED_EDGE ( 'NONE', *, *, #13374, .F. ) ;
#6693 = AXIS2_PLACEMENT_3D ( 'NONE', #3750, #8701, #13534 ) ;
#6694 = DIRECTION ( 'NONE',  ( 0.9510565162951500895, 0.3090169943749582204, 0.000000000000000000 ) ) ;
#6695 = ADVANCED_FACE ( 'NONE', ( #13766 ), #7647, .F. ) ;
#6696 =( NAMED_UNIT ( * ) SI_UNIT ( $, .STERADIAN. ) SOLID_ANGLE_UNIT ( ) );
#6697 =( REPRESENTATION_RELATIONSHIP ('NONE','NONE', #11191, #13925 ) REPRESENTATION_RELATIONSHIP_WITH_TRANSFORMATION ( #2006 )SHAPE_REPRESENTATION_RELATIONSHIP( ) );
#6698 = CARTESIAN_POINT ( 'NONE',  ( -2.066987299999999639, 0.8561741729129452860, -2.799999998907525267 ) ) ;
#6699 = ADVANCED_FACE ( 'NONE', ( #13532 ), #10042, .F. ) ;
#6700 = CARTESIAN_POINT ( 'NONE',  ( -0.2622916576875202743, 5.995491482261835259, 18.97384942646813144 ) ) ;
#6701 = CARTESIAN_POINT ( 'NONE',  ( -2.817313151351109823, -5.579000502529473771, 5.132341256341692137 ) ) ;
#6702 = CARTESIAN_POINT ( 'NONE',  ( -1.530808498934191571E-16, 2.500000000000000000, -0.1000000000000002554 ) ) ;
#6703 = CARTESIAN_POINT ( 'NONE',  ( 0.000000000000000000, 2.000000000000000000, 0.000000000000000000 ) ) ;
#6704 = CARTESIAN_POINT ( 'NONE',  ( -2.668367453516831134, 5.373994336898032742, 17.86763921416087797 ) ) ;
#6705 = DIRECTION ( 'NONE',  ( 0.000000000000000000, 0.000000000000000000, 1.000000000000000000 ) ) ;
#6706 = CARTESIAN_POINT ( 'NONE',  ( -5.931734679891428108, -0.9039278060245539148, 17.73617396794403689 ) ) ;
#6707 = AXIS2_PLACEMENT_3D ( 'NONE', #9555, #13284, #7479 ) ;
#6708 = CARTESIAN_POINT ( 'NONE',  ( 2.500000000000000444, 186.2999999978150356, 7.000000000000000000 ) ) ;
#6709 = ORIENTED_EDGE ( 'NONE', *, *, #15476, .T. ) ;
#6710 = ORIENTED_EDGE ( 'NONE', *, *, #14093, .F. ) ;
#6711 = VERTEX_POINT ( 'NONE', #2954 ) ;
#6712 = CARTESIAN_POINT ( 'NONE',  ( 3.253823204785093459, -5.337590213880519130, 18.87305891554299464 ) ) ;
#6713 = LINE ( 'NONE', #11704, #7086 ) ;
#6714 = EDGE_LOOP ( 'NONE', ( #4276, #2322, #9025, #5107 ) ) ;
#6715 = FILL_AREA_STYLE ('',( #15141 ) ) ;
#6716 = VECTOR ( 'NONE', #2458, 1000.000000000000114 ) ;
#6717 = CARTESIAN_POINT ( 'NONE',  ( -1.767766952966368432, -1.767766952966369320, 1.100000002184949643 ) ) ;
#6718 = CARTESIAN_POINT ( 'NONE',  ( -5.935543223013843850, -0.8771126767607685393, 31.00000000000000000 ) ) ;
#6719 = CARTESIAN_POINT ( 'NONE',  ( -2.500000000000000000, 0.000000000000000000, -2.300000000000000266 ) ) ;
#6720 = CARTESIAN_POINT ( 'NONE',  ( -1.965116437629976787E-16, 189.6999999978150697, 4.500000000000000000 ) ) ;
#6721 = CARTESIAN_POINT ( 'NONE',  ( 5.903347812666364547, -1.076697810262513322, 12.11397738943082736 ) ) ;
#6722 = CARTESIAN_POINT ( 'NONE',  ( 2.897581130414634077E-17, -9.750000000000003553, 2.000000000000001776 ) ) ;
#6723 = SHAPE_DEFINITION_REPRESENTATION ( #9705, #3059 ) ;
#6724 = FACE_BOUND ( 'NONE', #13051, .T. ) ;
#6725 = CARTESIAN_POINT ( 'NONE',  ( 2.500000000000000000, 189.5199999975965852, 8.035533905932739529 ) ) ;
#6726 = CARTESIAN_POINT ( 'NONE',  ( -2.913793338554793166E-15, 228.9118723800512782, 8.872930300147347182 ) ) ;
#6727 =( BOUNDED_CURVE ( )  B_SPLINE_CURVE ( 2, ( #8098, #3231, #1003, #8013, #6833, #4275, #15497, #4355, #4593 ),
 .UNSPECIFIED., .F., .F. ) 
 B_SPLINE_CURVE_WITH_KNOTS ( ( 3, 2, 2, 2, 3 ),
 ( 0.5714285714285713969, 0.5892857142857143016, 0.6071428571428570953, 0.6250000000000000000, 0.6428571428571429047 ),
 .UNSPECIFIED. ) 
 CURVE ( )  GEOMETRIC_REPRESENTATION_ITEM ( )  RATIONAL_B_SPLINE_CURVE ( ( 1.000000000000000000, 0.9238795325112867385, 1.000000000000000000, 0.9238795325112867385, 1.000000000000000000, 0.9238795325112867385, 1.000000000000000000, 0.9238795325112867385, 1.000000000000000000 ) ) 
 REPRESENTATION_ITEM ( '' )  );
#6728 = CARTESIAN_POINT ( 'NONE',  ( 3.568242062701418416, 5.132954954975583739, 19.00004906876532118 ) ) ;
#6729 = ADVANCED_FACE ( 'NONE', ( #9887 ), #5111, .F. ) ;
#6730 = EDGE_LOOP ( 'NONE', ( #7116, #82 ) ) ;
#6731 = CARTESIAN_POINT ( 'NONE',  ( -2.340099644010926294, -0.9261024465269158679, -2.500002477042004401 ) ) ;
#6732 = EDGE_LOOP ( 'NONE', ( #179, #14826, #3835, #963, #2308, #8288, #414, #13066, #8943, #5806, #1992, #3404, #3627, #4173, #12582, #11063 ) ) ;
#6733 = CARTESIAN_POINT ( 'NONE',  ( -3.159082487394895722, 5.393634094348264796, 17.20045537531157365 ) ) ;
#6734 = CARTESIAN_POINT ( 'NONE',  ( -2.500000000000000000, 0.000000000000000000, 0.2000000021849497878 ) ) ;
#6735 = CARTESIAN_POINT ( 'NONE',  ( 6.081590040723103385, 1.446205118472900786, 23.62632671364005787 ) ) ;
#6736 = ADVANCED_FACE ( 'NONE', ( #1516 ), #11305, .T. ) ;
#6737 = DIRECTION ( 'NONE',  ( 0.8090169943749510040, -0.5877852522924683631, 0.000000000000000000 ) ) ;
#6738 = DIRECTION ( 'NONE',  ( 0.000000000000000000, 0.000000000000000000, -1.000000000000000000 ) ) ;
#6739 = CARTESIAN_POINT ( 'NONE',  ( 1.767766952966369320, -1.767766952966368654, 2.000000000000000000 ) ) ;
#6740 = CARTESIAN_POINT ( 'NONE',  ( -1.035533905932738197, -2.500000000000000000, 0.2499999999999997780 ) ) ;
#6741 = CARTESIAN_POINT ( 'NONE',  ( 3.735808404764980661, 4.696639218303141128, 4.026019798777603853 ) ) ;
#6742 = SURFACE_STYLE_USAGE ( .BOTH. , #5151 ) ;
#6743 = CARTESIAN_POINT ( 'NONE',  ( 0.07711543383008488683, 0.4000000000000062395, -2.550194499910687362 ) ) ;
#6744 = CARTESIAN_POINT ( 'NONE',  ( -1.035533905932739751, 188.5500000000000114, 9.500000000000003553 ) ) ;
#6745 = AXIS2_PLACEMENT_3D ( 'NONE', #10202, #7965, #2880 ) ;
#6746 = CARTESIAN_POINT ( 'NONE',  ( 1.080575604060385553, 227.7131986584202821, 5.411092224208442936 ) ) ;
#6747 = FACE_OUTER_BOUND ( 'NONE', #138, .T. ) ;
#6748 = CARTESIAN_POINT ( 'NONE',  ( 0.9737725088284505670, 6.173885267451787229, 24.23735758726573053 ) ) ;
#6749 = CARTESIAN_POINT ( 'NONE',  ( 2.066987299999999639, 2.531329380823229670E-16, -2.349999998907525534 ) ) ;
#6750 = CARTESIAN_POINT ( 'NONE',  ( -1.035533905932737975, 187.4499999999999886, 4.500000000000000888 ) ) ;
#6751 = CARTESIAN_POINT ( 'NONE',  ( -2.841041022017575468, 5.567186575787166802, 24.76225281721715987 ) ) ;
#6753 = ORIENTED_EDGE ( 'NONE', *, *, #14160, .T. ) ;
#6752 = CARTESIAN_POINT ( 'NONE',  ( -0.1323602877610131345, -6.000000000000007105, 25.49999999999999645 ) ) ;
#6754 = DIRECTION ( 'NONE',  ( 0.000000000000000000, 1.000000000000000000, 0.000000000000000000 ) ) ;
#6755 = CIRCLE ( 'NONE', #15642, 1.500000000000001776 ) ;
#6756 = CARTESIAN_POINT ( 'NONE',  ( 5.665707375537505364, -1.979196487016587014, 16.99992038825522656 ) ) ;
#6757 = DIRECTION ( 'NONE',  ( 1.000000000000000000, 0.000000000000000000, 0.000000000000000000 ) ) ;
#6758 = CARTESIAN_POINT ( 'NONE',  ( -1.050085366295366640, 189.7133272379261086, 10.20285018932750631 ) ) ;
#6759 = DIRECTION ( 'NONE',  ( 0.000000000000000000, 0.000000000000000000, 1.000000000000000000 ) ) ;
#6760 = B_SPLINE_CURVE_WITH_KNOTS ( 'NONE', 3,
 ( #4106, #7920, #14929, #4021, #13805, #12842, #4343, #12692, #6510, #11654, #6741, #15014, #9131, #6664, #3147, #5233, #1867, #2914 ),
 .UNSPECIFIED., .F., .F.,
 ( 4, 2, 2, 2, 2, 2, 2, 2, 4 ),
 ( 0.003131918686235953941, 0.003523310662250245945, 0.003914702638264537515, 0.004306094614278829953, 0.004697486590293121524, 0.005088878566307413961, 0.005480270542321705532, 0.005871662518335997102, 0.006263054494350289540 ),
 .UNSPECIFIED. ) ;
#6761 = DIRECTION ( 'NONE',  ( -0.3090169943749447867, -0.9510565162951544194, 0.000000000000000000 ) ) ;
#6762 = FACE_OUTER_BOUND ( 'NONE', #3679, .T. ) ;
#6763 = CARTESIAN_POINT ( 'NONE',  ( 1.691241850060078322, 228.6046986201012601, 7.985794961368397615 ) ) ;
#6764 = CARTESIAN_POINT ( 'NONE',  ( 6.176542424588148172, -0.9554180641283416264, 24.36939309276500509 ) ) ;
#6765 = CARTESIAN_POINT ( 'NONE',  ( 0.02995359663100405703, 0.4000000000000062395, 2.524107975521145963 ) ) ;
#6766 = CARTESIAN_POINT ( 'NONE',  ( 0.09999999999998898659, 0.000000000000000000, 0.000000000000000000 ) ) ;
#6767 = ORIENTED_EDGE ( 'NONE', *, *, #1528, .F. ) ;
#6768 = CARTESIAN_POINT ( 'NONE',  ( 2.066987300000000971, 185.0999999989074922, 6.143825827087054492 ) ) ;
#6769 = CARTESIAN_POINT ( 'NONE',  ( 0.000000000000000000, 0.000000000000000000, 0.000000000000000000 ) ) ;
#6770 = EDGE_LOOP ( 'NONE', ( #3875, #4488, #10302, #261 ) ) ;
#6771 = CARTESIAN_POINT ( 'NONE',  ( 2.082642335314403343E-14, -6.250000000000000888, 31.00000000000000000 ) ) ;
#6772 = CARTESIAN_POINT ( 'NONE',  ( -4.005361199354941171, -4.468319061418822180, 4.199777826161208871 ) ) ;
#6773 = CARTESIAN_POINT ( 'NONE',  ( -3.011385983131281030, -5.190390249166461523, 5.799520541027148646 ) ) ;
#6774 = AXIS2_PLACEMENT_3D ( 'NONE', #1468, #2672, #4015 ) ;
#6775 = DIRECTION ( 'NONE',  ( 0.1736481776669307753, -0.9848077530122080203, -2.126576849575776229E-17 ) ) ;
#6776 = CARTESIAN_POINT ( 'NONE',  ( -0.8561741729129469514, 184.7999999989075093, 9.066987300000000971 ) ) ;
#6777 = CARTESIAN_POINT ( 'NONE',  ( 1.547212085679566958E-16, 22.00000000000000000, -11.25000000000000355 ) ) ;
#6778 = CARTESIAN_POINT ( 'NONE',  ( 1.035533905932739085, -2.500000000000000000, -0.4499999999999998446 ) ) ;
#6779 = LINE ( 'NONE', #4065, #1463 ) ;
#6780 = CARTESIAN_POINT ( 'NONE',  ( 3.000000000000000000, 3.673940397442059868E-16, 0.000000000000000000 ) ) ;
#6781 = EDGE_CURVE ( 'NONE', #12193, #10558, #2639, .T. ) ;
#6782 = CARTESIAN_POINT ( 'NONE',  ( -4.286401442266592809, 4.198423832313131321, 5.000000000000004441 ) ) ;
#6783 = CARTESIAN_POINT ( 'NONE',  ( -1.461580736456472351, -1.461580736456473018, -2.449999998907525178 ) ) ;
#6784 = CARTESIAN_POINT ( 'NONE',  ( -0.9739805876846552302, -5.920636045238190093, 18.26171386814421638 ) ) ;
#6785 = EDGE_CURVE ( 'NONE', #6298, #13541, #8198, .T. ) ;
#6786 = VERTEX_POINT ( 'NONE', #1594 ) ;
#6787 = ORIENTED_EDGE ( 'NONE', *, *, #5650, .F. ) ;
#6788 = CIRCLE ( 'NONE', #2963, 6.000000000000000000 ) ;
#6789 = ORIENTED_EDGE ( 'NONE', *, *, #15525, .F. ) ;
#6790 = DIRECTION ( 'NONE',  ( -0.000000000000000000, 1.000000000000000000, -0.000000000000000000 ) ) ;
#6791 = CARTESIAN_POINT ( 'NONE',  ( 3.673940397442060854E-16, 182.0000000000000000, 3.000000000000000888 ) ) ;
#6792 = ORIENTED_EDGE ( 'NONE', *, *, #13029, .T. ) ;
#6793 = PRODUCT_DEFINITION_SHAPE ( 'NONE', 'NONE',  #15759 ) ;
#6794 = CARTESIAN_POINT ( 'NONE',  ( -1.035533905932738197, -2.500000000000000000, -0.4499999978150506230 ) ) ;
#6795 = CARTESIAN_POINT ( 'NONE',  ( -2.817313151351206635, 5.579000502529421368, 31.00000000000000000 ) ) ;
#6796 = CARTESIAN_POINT ( 'NONE',  ( 2.930922878467330683, 5.520395124723648017, 25.00389213124970311 ) ) ;
#6797 = CARTESIAN_POINT ( 'NONE',  ( 0.8561741729129455081, 185.3999999989075604, 4.933012699999999029 ) ) ;
#6798 = CARTESIAN_POINT ( 'NONE',  ( -2.500000000000000000, -1.035533905932739307, 1.756999999978150484 ) ) ;
#6799 = CARTESIAN_POINT ( 'NONE',  ( -7.799024015210642702, -1.482594289697281020, 11.49999999999998224 ) ) ;
#6800 = EDGE_CURVE ( 'NONE', #13757, #2306, #14892, .T. ) ;
#6801 = SHAPE_DEFINITION_REPRESENTATION ( #4372, #13925 ) ;
#6802 = CARTESIAN_POINT ( 'NONE',  ( -2.066987299999999639, 0.000000000000000000, 1.250000001092474777 ) ) ;
#6803 = CARTESIAN_POINT ( 'NONE',  ( -2.500000000000000888, 188.4199999975965625, 8.035533905932737753 ) ) ;
#6804 = CARTESIAN_POINT ( 'NONE',  ( -1.312946155259101522, 228.7505583286450985, 8.407046118935697976 ) ) ;
#6805 = CARTESIAN_POINT ( 'NONE',  ( -8.185202263645752375E-31, 189.0000000000000000, -9.500000000000000000 ) ) ;
#6806 = ORIENTED_EDGE ( 'NONE', *, *, #7218, .T. ) ;
#6807 = CARTESIAN_POINT ( 'NONE',  ( -2.067846033730325495, 1.412380013906880283, -2.500797151967781851 ) ) ;
#6808 = CARTESIAN_POINT ( 'NONE',  ( -2.066987299999999195, -0.8561741729129467293, -0.8999999989075251339 ) ) ;
#6809 = ORIENTED_EDGE ( 'NONE', *, *, #8294, .T. ) ;
#6810 = CARTESIAN_POINT ( 'NONE',  ( -4.154121946521027731, 4.670585111242834486, 17.20112161576660981 ) ) ;
#6811 = CIRCLE ( 'NONE', #446, 1.499999999999999556 ) ;
#6812 = LINE ( 'NONE', #3291, #1259 ) ;
#6813 = CARTESIAN_POINT ( 'NONE',  ( 6.123233995736766282E-16, 6.000000000000000888, 6.000000000000005329 ) ) ;
#6814 = EDGE_LOOP ( 'NONE', ( #2491, #7019, #10115, #9800 ) ) ;
#6815 = LINE ( 'NONE', #15161, #2838 ) ;
#6816 = CARTESIAN_POINT ( 'NONE',  ( 6.123233995736766282E-16, -6.000000000000000888, 6.000000000000005329 ) ) ;
#6817 = CARTESIAN_POINT ( 'NONE',  ( 2.840966774240180293, -5.567223638426896493, 17.73809786915986564 ) ) ;
#6818 = CARTESIAN_POINT ( 'NONE',  ( 1.035533905932737531, 2.500000000000000444, -1.750000000000000222 ) ) ;
#6819 = CARTESIAN_POINT ( 'NONE',  ( 2.999999999999999556, 1.732050807568877859, -2.500000000000000000 ) ) ;
#6820 = CONICAL_SURFACE ( 'NONE', #9610, 2.575022672948154234, 0.08726646259971664044 ) ;
#6821 = DIRECTION ( 'NONE',  ( -1.000000000000000000, 0.000000000000000000, 0.000000000000000000 ) ) ;
#6822 = CARTESIAN_POINT ( 'NONE',  ( 2.500000000000000000, 187.9500000000000455, 8.035533905932739529 ) ) ;
#6823 = AXIS2_PLACEMENT_3D ( 'NONE', #1265, #9637, #12322 ) ;
#6824 = CARTESIAN_POINT ( 'NONE',  ( -1.619108980504621043, 228.6400225536183655, 8.087812496111112637 ) ) ;
#6825 = CARTESIAN_POINT ( 'NONE',  ( -2.897581130414634077E-17, 9.750000000000003553, 2.000000000000001776 ) ) ;
#6826 = ADVANCED_FACE ( 'NONE', ( #9013 ), #10197, .F. ) ;
#6827 = CARTESIAN_POINT ( 'NONE',  ( 0.8738239080081631194, 6.188820299975577477, 25.00355795710154894 ) ) ;
#6828 = CARTESIAN_POINT ( 'NONE',  ( -2.066987299999999639, 0.8561741729129455081, -2.799999998907524823 ) ) ;
#6829 = CARTESIAN_POINT ( 'NONE',  ( -1.767766952966369320, 187.5000000000000000, 5.232233047033630235 ) ) ;
#6830 = DIRECTION ( 'NONE',  ( 1.000000000000000000, -3.326610055774643275E-18, 1.062480551894329622E-17 ) ) ;
#6831 = ADVANCED_FACE ( 'NONE', ( #15047 ), #3900, .F. ) ;
#6832 = VECTOR ( 'NONE', #12213, 1000.000000000000000 ) ;
#6834 = ORIENTED_EDGE ( 'NONE', *, *, #12237, .F. ) ;
#6833 = CARTESIAN_POINT ( 'NONE',  ( -1.530808498934191571E-16, 2.500000000000000000, -1.599999997815050312 ) ) ;
#6835 = CARTESIAN_POINT ( 'NONE',  ( 0.4244143561419055910, 0.4000000000000062395, 2.581346380257589779 ) ) ;
#6836 = AXIS2_PLACEMENT_3D ( 'NONE', #22, #14580, #12031 ) ;
#6837 = CARTESIAN_POINT ( 'NONE',  ( -2.500000000000000444, 186.7999999999999829, 7.000000000000000000 ) ) ;
#6838 = CARTESIAN_POINT ( 'NONE',  ( -2.085029866008053734, 227.9837044594366375, 9.370153471119524013 ) ) ;
#6839 = DIRECTION ( 'NONE',  ( 0.8090169943749421222, 0.5877852522924802425, 0.000000000000000000 ) ) ;
#6840 = FACE_OUTER_BOUND ( 'NONE', #13234, .T. ) ;
#6841 = CARTESIAN_POINT ( 'NONE',  ( -1.939157702522992466, 228.0901138467679914, 6.499644785989321605 ) ) ;
#6842 = CARTESIAN_POINT ( 'NONE',  ( 1.637003574519428017, 228.6312591184326948, 8.062503195461440342 ) ) ;
#6844 = FACE_BOUND ( 'NONE', #10841, .T. ) ;
#6843 = CIRCLE ( 'NONE', #7096, 2.000000000000000000 ) ;
#6845 = CARTESIAN_POINT ( 'NONE',  ( 5.039986462824843482E-06, 0.4000000000000080158, 2.452138453183382971 ) ) ;
#6846 = PRESENTATION_LAYER_ASSIGNMENT (  '', '', ( #7844 ) ) ;
#6847 = CARTESIAN_POINT ( 'NONE',  ( 4.592425496802573972E-16, -2.500000000000000000, 1.200000002184949732 ) ) ;
#6848 = EDGE_LOOP ( 'NONE', ( #6323, #8209, #8615, #9688, #13071 ) ) ;
#6849 = CARTESIAN_POINT ( 'NONE',  ( -2.066987300000000527, 188.8499999989074922, 7.000000000000000000 ) ) ;
#6850 = CARTESIAN_POINT ( 'NONE',  ( 2.500000000000000444, 184.7999999999999829, 7.000000000000000000 ) ) ;
#6851 = VERTEX_POINT ( 'NONE', #12338 ) ;
#6852 = CARTESIAN_POINT ( 'NONE',  ( -2.668367453516813814, -5.373994336898041624, 24.49999999999999289 ) ) ;
#6853 =( GEOMETRIC_REPRESENTATION_CONTEXT ( 3 ) GLOBAL_UNCERTAINTY_ASSIGNED_CONTEXT ( ( #8565 ) ) GLOBAL_UNIT_ASSIGNED_CONTEXT ( ( #15417, #11985, #852 ) ) REPRESENTATION_CONTEXT ( 'NONE', 'WORKASPACE' ) );
#6854 = CARTESIAN_POINT ( 'NONE',  ( -3.420659742068393072, 4.931142898501730265, 31.99995053646223653 ) ) ;
#6855 = DIRECTION ( 'NONE',  ( -0.000000000000000000, 1.000000000000000000, -0.000000000000000000 ) ) ;
#6856 = CARTESIAN_POINT ( 'NONE',  ( -2.897581130414634077E-17, 9.750000000000003553, 2.000000000000001776 ) ) ;
#6857 = CARTESIAN_POINT ( 'NONE',  ( -0.5039005892418949584, 6.230833003620559474, 23.62636388911295171 ) ) ;
#6858 = CARTESIAN_POINT ( 'NONE',  ( 1.767766952966369320, -1.767766952966368654, -1.099999997815050312 ) ) ;
#6859 = CYLINDRICAL_SURFACE ( 'NONE', #11629, 1.000000000000000888 ) ;
#6860 = CARTESIAN_POINT ( 'NONE',  ( 0.000000000000000000, 229.2449477060184222, 9.834870838912449287 ) ) ;
#6861 = CARTESIAN_POINT ( 'NONE',  ( 2.500000000000000000, 3.061616997868383141E-16, 1.300000000000000044 ) ) ;
#6862 = CARTESIAN_POINT ( 'NONE',  ( -5.935543223013826086, -0.8771126767608832253, 17.99999999999998934 ) ) ;
#6863 = CARTESIAN_POINT ( 'NONE',  ( -0.6144377077728601089, -5.969178481556079774, 17.20033966857735663 ) ) ;
#6864 = ORIENTED_EDGE ( 'NONE', *, *, #842, .F. ) ;
#6865 = PRESENTATION_LAYER_ASSIGNMENT (  '', '', ( #15246 ) ) ;
#6866 = VERTEX_POINT ( 'NONE', #5032 ) ;
#6867 = ORIENTED_EDGE ( 'NONE', *, *, #9346, .F. ) ;
#6868 = CARTESIAN_POINT ( 'NONE',  ( 3.882809187878895507, -4.899079348630081654, 18.97400098023329562 ) ) ;
#6869 = CARTESIAN_POINT ( 'NONE',  ( 3.659182332138577465E-16, 220.7266909453316543, 6.312321839438380877 ) ) ;
#6870 = EDGE_LOOP ( 'NONE', ( #6069, #6481 ) ) ;
#6871 = CARTESIAN_POINT ( 'NONE',  ( 5.486982057989242101, -2.429327048029762626, 18.79931806258173665 ) ) ;
#6872 = EDGE_CURVE ( 'NONE', #3525, #10771, #5188, .T. ) ;
#6873 = CARTESIAN_POINT ( 'NONE',  ( 1.767766952966368654, 1.767766952966369098, -0.8999999978150504676 ) ) ;
#6874 = CARTESIAN_POINT ( 'NONE',  ( 0.2619456584322039094, -5.995505046955617701, 4.026071939286484103 ) ) ;
#6875 = AXIS2_PLACEMENT_3D ( 'NONE', #38, #8571, #13553 ) ;
#6876 = CARTESIAN_POINT ( 'NONE',  ( -3.882673863916208390, -4.899192824801000157, 4.025914576658296440 ) ) ;
#6877 = CARTESIAN_POINT ( 'NONE',  ( -2.500000000000000888, 189.1499999978150868, 8.035533905932737753 ) ) ;
#6878 = CARTESIAN_POINT ( 'NONE',  ( 1.035533905932737531, 2.500000000000000444, -0.1430000000218494827 ) ) ;
#6879 = CARTESIAN_POINT ( 'NONE',  ( 0.000000000000000000, 182.0000000000000000, 0.000000000000000000 ) ) ;
#6880 = PRODUCT_CONTEXT ( 'NONE', #3931, 'mechanical' ) ;
#6881 = CARTESIAN_POINT ( 'NONE',  ( 2.066987300000000083, -0.8561741729129449530, 1.600000001092474644 ) ) ;
#6882 = CARTESIAN_POINT ( 'NONE',  ( -5.935543223013847403, -0.8771126767607489993, 5.000000000000004441 ) ) ;
#6883 = CARTESIAN_POINT ( 'NONE',  ( 2.734462269239809729, 226.8914732116195125, 6.155466831691636109 ) ) ;
#6884 = CARTESIAN_POINT ( 'NONE',  ( 2.500000000000000000, 3.061616997868383141E-16, 0.6000000021849497545 ) ) ;
#6885 = ORIENTED_EDGE ( 'NONE', *, *, #12497, .F. ) ;
#6886 = CARTESIAN_POINT ( 'NONE',  ( 3.421280866381210650, -4.930711975950862858, 3.999950679266884634 ) ) ;
#6887 = EDGE_LOOP ( 'NONE', ( #6166, #7198, #10988, #6787, #8708 ) ) ;
#6888 = CARTESIAN_POINT ( 'NONE',  ( -3.459447313391952328, 5.206669755180917569, 17.02599901976669017 ) ) ;
#6889 = EDGE_CURVE ( 'NONE', #478, #4153, #5468, .T. ) ;
#6890 = FACE_OUTER_BOUND ( 'NONE', #10516, .T. ) ;
#6891 = CARTESIAN_POINT ( 'NONE',  ( 5.558508435838283468, 2.857531096718751051, 24.36762589283694425 ) ) ;
#6892 = VERTEX_POINT ( 'NONE', #12801 ) ;
#6893 = CARTESIAN_POINT ( 'NONE',  ( -3.000000000000000000, 1.732050807568877415, -2.500000000000000000 ) ) ;
#6894 = FACE_BOUND ( 'NONE', #2435, .T. ) ;
#6895 = CARTESIAN_POINT ( 'NONE',  ( 2.996417732210528762, -5.485687819086929373, 17.38603820591928439 ) ) ;
#6896 = CARTESIAN_POINT ( 'NONE',  ( -1.767766952966369098, 1.767766952966369098, -1.600000000000000311 ) ) ;
#6897 = DIRECTION ( 'NONE',  ( 0.000000000000000000, 0.000000000000000000, 1.000000000000000000 ) ) ;
#6898 = EDGE_CURVE ( 'NONE', #15036, #398, #10950, .T. ) ;
#6899 = DIRECTION ( 'NONE',  ( 0.000000000000000000, 0.000000000000000000, 1.000000000000000000 ) ) ;
#6900 = PRODUCT ( 'silicon body', 'silicon body', '', ( #6880 ) ) ;
#6901 = CARTESIAN_POINT ( 'NONE',  ( 0.000000000000000000, 0.000000000000000000, 2.500000000000000000 ) ) ;
#6902 = CARTESIAN_POINT ( 'NONE',  ( -1.035533905932737753, 185.7499999978150527, 4.500000000000000888 ) ) ;
#6903 = CARTESIAN_POINT ( 'NONE',  ( -1.052533753945321227, 228.8137749680355455, 8.589619379135912780 ) ) ;
#6904 = DIRECTION ( 'NONE',  ( 1.000000000000000000, 0.000000000000000000, 0.000000000000000000 ) ) ;
#6905 = CARTESIAN_POINT ( 'NONE',  ( 2.031800924094035195E-13, 6.250000000000000888, 23.49999999999999289 ) ) ;
#6906 = CARTESIAN_POINT ( 'NONE',  ( -1.265664690411614835E-16, 2.066987299999999639, -2.949999998907525178 ) ) ;
#6907 = CARTESIAN_POINT ( 'NONE',  ( 1.767766952966369320, 185.7000000000000171, 5.232233047033630235 ) ) ;
#6908 = CARTESIAN_POINT ( 'NONE',  ( -2.500000000000000444, 187.4499999978150981, 5.964466094067261359 ) ) ;
#6910 = ORIENTED_EDGE ( 'NONE', *, *, #14100, .T. ) ;
#6909 = DIRECTION ( 'NONE',  ( 0.000000000000000000, 0.000000000000000000, 1.000000000000000000 ) ) ;
#6911 = CARTESIAN_POINT ( 'NONE',  ( -5.648794263291730289, 2.676232015153646504, 18.61441947245482709 ) ) ;
#6912 = ORIENTED_EDGE ( 'NONE', *, *, #9889, .T. ) ;
#6913 = EDGE_CURVE ( 'NONE', #10984, #2248, #3255, .T. ) ;
#6914 = FACE_OUTER_BOUND ( 'NONE', #8157, .T. ) ;
#6915 = CARTESIAN_POINT ( 'NONE',  ( -1.815463298294986760, 226.5191110010208035, 5.058303205087121945 ) ) ;
#6916 = CARTESIAN_POINT ( 'NONE',  ( 5.558508435838322548, -2.857531096718671115, 24.49999999999999289 ) ) ;
#6917 = CARTESIAN_POINT ( 'NONE',  ( -5.421010862427522170E-16, 185.3300000002185186, 9.500000000000001776 ) ) ;
#6918 = CARTESIAN_POINT ( 'NONE',  ( 5.131373506000584506, 7.062729720844102665, 31.00000000000000000 ) ) ;
#6919 = CARTESIAN_POINT ( 'NONE',  ( 1.939628903789791359, 228.4085481513286311, 7.419301219863100982 ) ) ;
#6920 = EDGE_CURVE ( 'NONE', #5611, #13777, #3031, .T. ) ;
#6921 = CARTESIAN_POINT ( 'NONE',  ( 2.500000000000000000, 3.061616997868383141E-16, -1.900000000000000133 ) ) ;
#6922 = CARTESIAN_POINT ( 'NONE',  ( 0.08707474757428863843, 0.4000000000000061839, 2.551476655618785561 ) ) ;
#6923 = VECTOR ( 'NONE', #4421, 1000.000000000000000 ) ;
#6924 = CARTESIAN_POINT ( 'NONE',  ( -9.750000000000003553, 184.0000000000000000, -1.500000000000033751 ) ) ;
#6925 = ORIENTED_EDGE ( 'NONE', *, *, #14615, .T. ) ;
#6926 = CARTESIAN_POINT ( 'NONE',  ( 1.461580736456472795, 189.3499999989074922, 5.538419263543527649 ) ) ;
#6927 = CARTESIAN_POINT ( 'NONE',  ( 3.419318284370212790, 4.932111238568167799, 30.00007997643738022 ) ) ;
#6928 = VERTEX_POINT ( 'NONE', #6777 ) ;
#6929 = CARTESIAN_POINT ( 'NONE',  ( -1.035533905932739751, 186.1500000000000057, 9.500000000000000000 ) ) ;
#6930 = ADVANCED_FACE ( 'NONE', ( #6624 ), #9090, .F. ) ;
#6931 = CIRCLE ( 'NONE', #2603, 6.250000000000000888 ) ;
#6932 = CARTESIAN_POINT ( 'NONE',  ( -3.311384659207154968, 5.004923837169406475, 31.97358595436693918 ) ) ;
#6933 = DIRECTION ( 'NONE',  ( -0.000000000000000000, 1.000000000000000000, -0.000000000000000000 ) ) ;
#6934 = CARTESIAN_POINT ( 'NONE',  ( 1.461580736456473240, 187.5499999989075093, 5.538419263543526760 ) ) ;
#6935 = DIRECTION ( 'NONE',  ( -0.3090169943749447867, -0.9510565162951544194, 0.000000000000000000 ) ) ;
#6936 = CARTESIAN_POINT ( 'NONE',  ( 1.767766952966368654, 1.767766952966369098, 0.7000000021849498433 ) ) ;
#6937 = LINE ( 'NONE', #14229, #9612 ) ;
#6938 = CARTESIAN_POINT ( 'NONE',  ( -1.768235190473915752, 189.0000319710720191, 5.232701284541176001 ) ) ;
#6939 = CARTESIAN_POINT ( 'NONE',  ( 2.996417732210555851, 5.485687819086916051, 31.61396179408072626 ) ) ;
#6940 = CARTESIAN_POINT ( 'NONE',  ( 5.317509234263941842, 2.779225709351030638, 31.00000000000000000 ) ) ;
#6941 = EDGE_LOOP ( 'NONE', ( #14029, #11527, #2634, #13235 ) ) ;
#6942 = AXIS2_PLACEMENT_3D ( 'NONE', #1301, #116, #4981 ) ;
#6943 = ORIENTED_EDGE ( 'NONE', *, *, #788, .T. ) ;
#6944 = B_SPLINE_CURVE_WITH_KNOTS ( 'NONE', 3,
 ( #13324, #10862, #6101, #10943, #4907, #8168, #11888, #7053, #11810, #10630, #15492, #11020, #120, #7367, #12209, #13404, #6182, #2514 ),
 .UNSPECIFIED., .F., .F.,
 ( 4, 2, 2, 2, 2, 2, 2, 2, 4 ),
 ( 0.000000000000000000, 0.0003914898357794942426, 0.0007829796715589884852, 0.001174469507338482674, 0.001565959343117976970, 0.001957449178897471918, 0.002348939014676966648, 0.002740428850456461812, 0.003131918686235956543 ),
 .UNSPECIFIED. ) ;
#6945 = ORIENTED_EDGE ( 'NONE', *, *, #7757, .T. ) ;
#6946 = CARTESIAN_POINT ( 'NONE',  ( -0.8561741729129455081, 185.4999999989075263, 4.933012699999999029 ) ) ;
#6947 = CARTESIAN_POINT ( 'NONE',  ( -2.782713018890709211, 5.315928322779123860, 12.00439760644213294 ) ) ;
#6948 = ORIENTED_EDGE ( 'NONE', *, *, #7108, .F. ) ;
#6949 = CARTESIAN_POINT ( 'NONE',  ( -1.035533905932738197, -2.500000000000000000, 1.150000002184949466 ) ) ;
#6950 = CARTESIAN_POINT ( 'NONE',  ( 0.9735856429312852445, -5.920699391845026582, 5.262852839067273081 ) ) ;
#6951 = CYLINDRICAL_SURFACE ( 'NONE', #11523, 3.000000000000000000 ) ;
#6952 = CARTESIAN_POINT ( 'NONE',  ( -2.066987300000000083, 184.8499999989075206, 7.000000000000000000 ) ) ;
#6953 = CARTESIAN_POINT ( 'NONE',  ( -2.500000000000000444, 1.035533905932737753, 0.8569999999781505728 ) ) ;
#6954 = CARTESIAN_POINT ( 'NONE',  ( 6.176542424588118863, -0.9554180641285446862, 5.000000000000004441 ) ) ;
#6955 = ITEM_DEFINED_TRANSFORMATION ( 'NONE', 'NONE', #6875,  #14201 ) ;
#6956 = B_SPLINE_CURVE_WITH_KNOTS ( 'NONE', 3,
 ( #13418, #13642, #14852, #3632, #12146, #6434, #12375, #11266, #6354, #8508, #11188, #287, #4996, #5150, #2596, #11109, #1245, #11032 ),
 .UNSPECIFIED., .F., .F.,
 ( 4, 2, 2, 2, 2, 2, 2, 2, 4 ),
 ( 0.003131486019301991160, 0.003522824630466697866, 0.003914163241631404139, 0.004305501852796111278, 0.004696840463960817551, 0.005088179075125523823, 0.005479517686290230963, 0.005870856297454938102, 0.006262194908619644375 ),
 .UNSPECIFIED. ) ;
#6957 = CARTESIAN_POINT ( 'NONE',  ( 4.344313232727172291, -4.493553492990049136, 4.495630303198468347 ) ) ;
#6958 = CARTESIAN_POINT ( 'NONE',  ( 1.586671692599169736, 226.4708623422775418, 4.916117818249839289 ) ) ;
#6959 = CYLINDRICAL_SURFACE ( 'NONE', #7242, 2.500000000000000000 ) ;
#6960 = ORIENTED_EDGE ( 'NONE', *, *, #11823, .F. ) ;
#6961 = CARTESIAN_POINT ( 'NONE',  ( -5.330004929009523273, 2.755647751839523707, 24.76239891805597537 ) ) ;
#6962 = CIRCLE ( 'NONE', #93, 1.500000000000000222 ) ;
#6963 = ORIENTED_EDGE ( 'NONE', *, *, #6872, .T. ) ;
#6964 = CARTESIAN_POINT ( 'NONE',  ( -6.105861027178926648, 1.337741388557089461, 25.29954462468842991 ) ) ;
#6965 = LINE ( 'NONE', #15314, #9626 ) ;
#6966 = DIRECTION ( 'NONE',  ( 0.000000000000000000, 0.000000000000000000, 1.000000000000000000 ) ) ;
#6967 = EDGE_LOOP ( 'NONE', ( #12179, #3006 ) ) ;
#6968 = DIRECTION ( 'NONE',  ( -1.000000000000000000, 0.000000000000000000, 0.000000000000000000 ) ) ;
#6969 = CARTESIAN_POINT ( 'NONE',  ( -5.940390500375658078, 6.474944468551550258, 5.000000000000004441 ) ) ;
#6970 = CARTESIAN_POINT ( 'NONE',  ( 1.767766952966369320, -1.767766952966368654, -1.099999997815050312 ) ) ;
#6971 = CARTESIAN_POINT ( 'NONE',  ( -1.767766952966368432, -1.767766952966369320, 0.2000000000000000944 ) ) ;
#6972 = CARTESIAN_POINT ( 'NONE',  ( -4.290821322214476652, -4.545321419741457980, 25.11441947245483419 ) ) ;
#6973 = DIRECTION ( 'NONE',  ( 0.000000000000000000, 0.000000000000000000, 1.000000000000000000 ) ) ;
#6974 = CARTESIAN_POINT ( 'NONE',  ( 0.004861884284635707709, 0.4000000000000062395, -2.484217348758675392 ) ) ;
#6975 = CARTESIAN_POINT ( 'NONE',  ( -2.500000000000000444, 185.1499999978150584, 8.035533905932737753 ) ) ;
#6976 = EDGE_CURVE ( 'NONE', #3914, #11745, #7350, .T. ) ;
#6977 = CARTESIAN_POINT ( 'NONE',  ( -1.958673816210946272, 228.3772695101851014, 7.328966720224260101 ) ) ;
#6978 = CARTESIAN_POINT ( 'NONE',  ( 2.692143549875383179, 5.362363179736484575, 31.26194324003146718 ) ) ;
#6979 = CARTESIAN_POINT ( 'NONE',  ( 0.1323408341374962827, 6.250000000000000888, 25.50000000000002132 ) ) ;
#6980 = EDGE_CURVE ( 'NONE', #10964, #13817, #15203, .T. ) ;
#6981 = CIRCLE ( 'NONE', #6227, 1.500000000000000000 ) ;
#6982 = CARTESIAN_POINT ( 'NONE',  ( -1.623479154671611857, 188.9999999998642295, 5.090171998070187165 ) ) ;
#6983 = CARTESIAN_POINT ( 'NONE',  ( -1.035533905932739751, 188.5500000000000114, 9.500000000000003553 ) ) ;
#6984 = CARTESIAN_POINT ( 'NONE',  ( 2.930600586412863251, -5.520563544161807279, 25.00308643866044989 ) ) ;
#6985 = EDGE_CURVE ( 'NONE', #721, #8233, #8306, .T. ) ;
#6987 = ORIENTED_EDGE ( 'NONE', *, *, #14060, .F. ) ;
#6986 = DIRECTION ( 'NONE',  ( -1.062480551894329930E-17, -2.775557561562888393E-16, 1.000000000000000000 ) ) ;
#6988 = DIRECTION ( 'NONE',  ( -0.000000000000000000, 1.000000000000000000, -0.000000000000000000 ) ) ;
#6989 = CYLINDRICAL_SURFACE ( 'NONE', #15456, 1.000000000000000666 ) ;
#6990 = CARTESIAN_POINT ( 'NONE',  ( -2.998365736231170420, 227.3239176724307811, 7.428857950662880683 ) ) ;
#6991 = CARTESIAN_POINT ( 'NONE',  ( 1.543908090016931078, 189.4216793162960357, 4.413729295337608605 ) ) ;
#6992 = CARTESIAN_POINT ( 'NONE',  ( 4.743384504624081899E-17, 185.7300000002184959, 4.500000000000000000 ) ) ;
#6993 = CARTESIAN_POINT ( 'NONE',  ( -3.158825713737527963, 5.393784879207143668, 5.799331489075775004 ) ) ;
#6994 =( REPRESENTATION_RELATIONSHIP ('NONE','NONE', #11191, #4596 ) REPRESENTATION_RELATIONSHIP_WITH_TRANSFORMATION ( #13059 )SHAPE_REPRESENTATION_RELATIONSHIP( ) );
#6995 = CARTESIAN_POINT ( 'NONE',  ( 1.314367061980813878, 227.7707019980692564, 5.577165148888615143 ) ) ;
#6996 = FACE_OUTER_BOUND ( 'NONE', #1698, .T. ) ;
#6997 = LINE ( 'NONE', #10494, #12861 ) ;
#6998 = DIRECTION ( 'NONE',  ( -0.5877852522924685852, -0.8090169943749507819, 0.000000000000000000 ) ) ;
#6999 = EDGE_LOOP ( 'NONE', ( #14469, #10592, #9420, #8536 ) ) ;
#7000 = CARTESIAN_POINT ( 'NONE',  ( 0.8561741729129458411, 184.3999999989075036, 4.933012699999999029 ) ) ;
#7001 = STYLED_ITEM ( 'NONE', ( #832 ), #10455 ) ;
#7002 = ORIENTED_EDGE ( 'NONE', *, *, #923, .T. ) ;
#7003 = FACE_OUTER_BOUND ( 'NONE', #11952, .T. ) ;
#7004 = CARTESIAN_POINT ( 'NONE',  ( 4.322356511625595310, 7.650514973136599117, 11.49999999999998224 ) ) ;
#7005 = CARTESIAN_POINT ( 'NONE',  ( -5.935543223013836744, -0.8771126767608161678, 11.49999999999998224 ) ) ;
#7006 = CARTESIAN_POINT ( 'NONE',  ( -2.066987300000000971, 187.8499999989074922, 7.000000000000000000 ) ) ;
#7007 = CARTESIAN_POINT ( 'NONE',  ( 3.311576095066539160, -5.004818610361334130, 18.97377823943292086 ) ) ;
#7008 = ADVANCED_FACE ( 'NONE', ( #948 ), #3574, .F. ) ;
#7009 = CARTESIAN_POINT ( 'NONE',  ( -2.500000000000000000, 0.000000000000000000, -0.5999999978150503122 ) ) ;
#7010 = CARTESIAN_POINT ( 'NONE',  ( -6.250000000000000888, 0.000000000000000000, 0.000000000000000000 ) ) ;
#7011 = CARTESIAN_POINT ( 'NONE',  ( -5.999999999999999112, 194.5935680195190116, 12.11154058223188379 ) ) ;
#7012 = VECTOR ( 'NONE', #8002, 1000.000000000000114 ) ;
#7013 = CARTESIAN_POINT ( 'NONE',  ( 0.6151877315910210253, -6.220340188096013634, 31.79906673469668732 ) ) ;
#7014 = CARTESIAN_POINT ( 'NONE',  ( 3.159612573729224216, 5.393342049074633771, 31.80026515017676658 ) ) ;
#7015 = CARTESIAN_POINT ( 'NONE',  ( 2.500000000000000444, 184.0000000000000000, 7.000000000000000000 ) ) ;
#7016 = ORIENTED_EDGE ( 'NONE', *, *, #4161, .F. ) ;
#7017 = EDGE_CURVE ( 'NONE', #11546, #9142, #10392, .T. ) ;
#7018 = EDGE_LOOP ( 'NONE', ( #1443, #15390, #11449, #392 ) ) ;
#7019 = ORIENTED_EDGE ( 'NONE', *, *, #9903, .F. ) ;
#7020 = DIRECTION ( 'NONE',  ( -0.8660254037844385966, 0.5000000000000001110, 0.000000000000000000 ) ) ;
#7021 = DIRECTION ( 'NONE',  ( -0.3090169943749446202, -0.9510565162951544194, 0.000000000000000000 ) ) ;
#7022 = EDGE_CURVE ( 'NONE', #727, #12035, #8111, .T. ) ;
#7023 = CIRCLE ( 'NONE', #2952, 1.499999999999999556 ) ;
#7024 = ORIENTED_EDGE ( 'NONE', *, *, #9248, .T. ) ;
#7025 = CARTESIAN_POINT ( 'NONE',  ( -2.500000000000000000, 0.000000000000000000, -1.399999997815050579 ) ) ;
#7026 = CARTESIAN_POINT ( 'NONE',  ( -0.8002302970944432658, 5.947135855825893991, 23.88601773212297630 ) ) ;
#7027 = LINE ( 'NONE', #8059, #7216 ) ;
#7028 = CARTESIAN_POINT ( 'NONE',  ( -2.066987300000000971, 184.8999999989075320, 7.856174172912944620 ) ) ;
#7029 = CARTESIAN_POINT ( 'NONE',  ( 1.767766952966369320, -1.767766952966368654, -0.3930000000218496492 ) ) ;
#7030 = CARTESIAN_POINT ( 'NONE',  ( 6.021135683317697662, -1.680226122398213340, 4.026227171247320769 ) ) ;
#7031 = CARTESIAN_POINT ( 'NONE',  ( -1.461580736456472795, 1.461580736456472795, -0.4499999989075252338 ) ) ;
#7032 = CARTESIAN_POINT ( 'NONE',  ( 3.159612573729294827, -5.393342049074592026, 30.19973484982324408 ) ) ;
#7033 = CARTESIAN_POINT ( 'NONE',  ( 2.975657739721877970, 227.4162173224905530, 7.700537803285528504 ) ) ;
#7034 = CONICAL_SURFACE ( 'NONE', #424, 4.000000000000001776, 0.1745329251994333364 ) ;
#7035 = CARTESIAN_POINT ( 'NONE',  ( 3.459597053047735127, 5.206576120509819106, 18.97408542334169823 ) ) ;
#7036 = ORIENTED_EDGE ( 'NONE', *, *, #1067, .F. ) ;
#7037 = CARTESIAN_POINT ( 'NONE',  ( -5.620879908643923173, 2.102487719022013479, 25.47377823943293862 ) ) ;
#7038 = EDGE_LOOP ( 'NONE', ( #14506, #4949, #8692, #13933 ) ) ;
#7039 = VERTEX_POINT ( 'NONE', #441 ) ;
#7040 = CARTESIAN_POINT ( 'NONE',  ( -5.615811513734953131, 2.743665920700568250, 25.00308643866045344 ) ) ;
#7041 = DIRECTION ( 'NONE',  ( 1.000000000000000000, 0.000000000000000000, 0.000000000000000000 ) ) ;
#7042 = EDGE_LOOP ( 'NONE', ( #5921, #2126 ) ) ;
#7043 = CARTESIAN_POINT ( 'NONE',  ( 3.419318284370244765, -4.932111238568142930, 12.49992002356259668 ) ) ;
#7044 = CARTESIAN_POINT ( 'NONE',  ( 5.330189595673701319, -2.755293208590119836, 17.73617396794405821 ) ) ;
#7045 = DIRECTION ( 'NONE',  ( 0.000000000000000000, 1.000000000000000000, 0.000000000000000000 ) ) ;
#7046 = DIRECTION ( 'NONE',  ( -0.000000000000000000, 1.000000000000000000, -0.000000000000000000 ) ) ;
#7047 = CARTESIAN_POINT ( 'NONE',  ( -6.176542424588072677, -0.9554180641288341214, 24.49999999999999289 ) ) ;
#7048 = CARTESIAN_POINT ( 'NONE',  ( 1.547212085679566958E-16, 19.99999999999999645, -11.25000000000000355 ) ) ;
#7049 = CARTESIAN_POINT ( 'NONE',  ( 0.08820272154344555027, 0.4000000000000062395, -2.551527784092946227 ) ) ;
#7050 = PRODUCT_DEFINITION_SHAPE ( 'NONE', 'NONE',  #15764 ) ;
#7051 = CARTESIAN_POINT ( 'NONE',  ( 1.035533905932738197, 188.6499999999999773, 9.500000000000003553 ) ) ;
#7052 = CARTESIAN_POINT ( 'NONE',  ( -0.4531526159469659309, 228.8951261137066524, 8.824566127799945647 ) ) ;
#7053 = CARTESIAN_POINT ( 'NONE',  ( 5.620786884546286721, 2.102685372472903769, 10.52641404563305016 ) ) ;
#7054 = VECTOR ( 'NONE', #14596, 1000.000000000000000 ) ;
#7055 = CARTESIAN_POINT ( 'NONE',  ( 5.665707375537437862, 1.979196487016773975, 32.00007961174475923 ) ) ;
#7056 = ORIENTED_EDGE ( 'NONE', *, *, #13222, .T. ) ;
#7057 = DIRECTION ( 'NONE',  ( -0.9510565162951544194, 0.3090169943749447312, 0.000000000000000000 ) ) ;
#7058 = CARTESIAN_POINT ( 'NONE',  ( 6.768587589771821120E-14, -6.250000000000000888, 11.49999999999998224 ) ) ;
#7060 = EDGE_LOOP ( 'NONE', ( #13678, #11045, #12505, #12269, #2349, #13673, #9191, #8601, #625, #2143, #3623, #6244, #5436, #10825, #14156 ) ) ;
#7059 = CARTESIAN_POINT ( 'NONE',  ( -0.8738118504723636493, -5.936246475285062552, 25.00357242174242245 ) ) ;
#7061 = DIRECTION ( 'NONE',  ( 0.5877852522924802425, -0.8090169943749422332, 0.000000000000000000 ) ) ;
#7062 = FACE_OUTER_BOUND ( 'NONE', #8378, .T. ) ;
#7063 = CARTESIAN_POINT ( 'NONE',  ( 0.000000000000000000, 0.000000000000000000, 0.000000000000000000 ) ) ;
#7064 = EDGE_CURVE ( 'NONE', #10038, #15573, #14555, .T. ) ;
#7065 = VECTOR ( 'NONE', #2937, 1000.000000000000114 ) ;
#7066 = CYLINDRICAL_SURFACE ( 'NONE', #3762, 6.000000000000000000 ) ;
#7067 = CARTESIAN_POINT ( 'NONE',  ( -2.228027794420240681, 226.6433447131122989, 5.424436590844790018 ) ) ;
#7068 = CARTESIAN_POINT ( 'NONE',  ( 5.558508435838283468, 2.857531096718750607, 24.49999999999999289 ) ) ;
#7069 = FACE_OUTER_BOUND ( 'NONE', #8373, .T. ) ;
#7070 = CARTESIAN_POINT ( 'NONE',  ( -1.739661649193494419, 228.5884852582535700, 7.938969847602396435 ) ) ;
#7071 = CARTESIAN_POINT ( 'NONE',  ( -1.974809306405319154, 228.1756194782155944, 6.746589926531873616 ) ) ;
#7072 = CARTESIAN_POINT ( 'NONE',  ( 6.176542424588115310, 0.9554180641285648923, 11.49999999999998224 ) ) ;
#7073 = CARTESIAN_POINT ( 'NONE',  ( -0.8561741729129458411, -2.066987299999999195, 0.8000000010924748217 ) ) ;
#7074 = CARTESIAN_POINT ( 'NONE',  ( -4.267992336621142080, -4.217442018460050512, 30.73805675996852216 ) ) ;
#7075 = ORIENTED_EDGE ( 'NONE', *, *, #11333, .F. ) ;
#7076 = DIRECTION ( 'NONE',  ( 1.000000000000000000, -3.326610055774637112E-18, -1.062480551894331163E-17 ) ) ;
#7077 = AXIS2_PLACEMENT_3D ( 'NONE', #15174, #10402, #12702 ) ;
#7078 = CARTESIAN_POINT ( 'NONE',  ( 3.659182332138073087E-16, 190.0875178197511275, 4.201689379953569947 ) ) ;
#7079 = ORIENTED_EDGE ( 'NONE', *, *, #9722, .T. ) ;
#7080 = FACE_OUTER_BOUND ( 'NONE', #11718, .T. ) ;
#7081 = ADVANCED_FACE ( 'NONE', ( #8202, #2777, #14721, #3809, #6290, #3882 ), #8682, .T. ) ;
#7082 = DIRECTION ( 'NONE',  ( 0.9961946980917455452, -1.683102924354769481E-17, 0.08715574274765841567 ) ) ;
#7083 = CARTESIAN_POINT ( 'NONE',  ( 2.066987300000000083, 184.4499999989075150, 7.000000000000000000 ) ) ;
#7084 = CARTESIAN_POINT ( 'NONE',  ( 5.375886393124394758, 2.665038680141264216, 17.49560239355787417 ) ) ;
#7085 = CARTESIAN_POINT ( 'NONE',  ( -2.066987300000000527, 186.1999999989075150, 6.143825827087054492 ) ) ;
#7086 = VECTOR ( 'NONE', #10519, 1000.000000000000000 ) ;
#7087 = CARTESIAN_POINT ( 'NONE',  ( 2.668367453516506504, 5.373994336898192614, 17.99999999999998934 ) ) ;
#7088 = CARTESIAN_POINT ( 'NONE',  ( -1.035533905932738197, -2.500000000000000000, -0.4499999978150504010 ) ) ;
#7089 = DIRECTION ( 'NONE',  ( 0.000000000000000000, 0.000000000000000000, -1.000000000000000000 ) ) ;
#7090 = CARTESIAN_POINT ( 'NONE',  ( 0.000000000000000000, 194.5935680195190116, 12.11154058223188201 ) ) ;
#7091 = CARTESIAN_POINT ( 'NONE',  ( -5.935543223013850955, 0.8771126767607324570, 11.49999999999998224 ) ) ;
#7092 = CARTESIAN_POINT ( 'NONE',  ( 5.746619684944255901, 1.730157667110902242, 3.999950679266886855 ) ) ;
#7093 = DIRECTION ( 'NONE',  ( 0.8090169943749506709, -0.5877852522924686962, 0.000000000000000000 ) ) ;
#7094 = VERTEX_POINT ( 'NONE', #5252 ) ;
#7095 = ORIENTED_EDGE ( 'NONE', *, *, #8766, .F. ) ;
#7096 = AXIS2_PLACEMENT_3D ( 'NONE', #9920, #10156, #8970 ) ;
#7097 = ORIENTED_EDGE ( 'NONE', *, *, #6211, .T. ) ;
#7098 = CARTESIAN_POINT ( 'NONE',  ( -1.461580736456473240, 184.9499999989075150, 8.461580736456472351 ) ) ;
#7099 = CARTESIAN_POINT ( 'NONE',  ( -3.011139120916598078, 5.190534000030295303, 12.29931806258173843 ) ) ;
#7100 = ORIENTED_EDGE ( 'NONE', *, *, #9159, .T. ) ;
#7101 = CARTESIAN_POINT ( 'NONE',  ( -2.500000000000000000, -1.035533905932739307, -1.349999997815050312 ) ) ;
#7102 = CARTESIAN_POINT ( 'NONE',  ( 7.347880347650999152E-16, -6.000000000000000888, 4.000000000000004441 ) ) ;
#7103 = B_SPLINE_CURVE_WITH_KNOTS ( 'NONE', 3,
 ( #2346, #12133, #14351, #8248, #14270, #2107, #2182, #13084, #5860, #4666, #4745, #9764, #913, #3380, #8497, #10785, #4588, #3305 ),
 .UNSPECIFIED., .F., .F.,
 ( 4, 2, 2, 2, 2, 2, 2, 2, 4 ),
 ( 0.000000000000000000, 0.0003914357524127490035, 0.0007828715048254980069, 0.001174307257238247065, 0.001565743009650996014, 0.001957178762063744963, 0.002348614514476494129, 0.002740050266889242862, 0.003131486019301992028 ),
 .UNSPECIFIED. ) ;
#7104 = CYLINDRICAL_SURFACE ( 'NONE', #5653, 1.500000000000001776 ) ;
#7105 = CARTESIAN_POINT ( 'NONE',  ( 2.066987300000000083, 186.8999999989075036, 6.143825827087054492 ) ) ;
#7106 = EDGE_CURVE ( 'NONE', #398, #15036, #5631, .T. ) ;
#7107 = CARTESIAN_POINT ( 'NONE',  ( -2.500000000000000444, 1.035533905932737753, 0.05699999997815063946 ) ) ;
#7108 = EDGE_CURVE ( 'NONE', #10844, #12887, #4609, .T. ) ;
#7109 = CARTESIAN_POINT ( 'NONE',  ( 5.770288754215126659, -2.404361317819967869, 4.126180359549290522 ) ) ;
#7110 = ITEM_DEFINED_TRANSFORMATION ( 'NONE', 'NONE', #6119,  #14201 ) ;
#7111 = CARTESIAN_POINT ( 'NONE',  ( 1.035533905932737753, 188.9499999999999886, 4.500000000000000888 ) ) ;
#7112 = CARTESIAN_POINT ( 'NONE',  ( 2.817313151351170220, -5.579000502529441796, 30.86936067245787285 ) ) ;
#7113 = CARTESIAN_POINT ( 'NONE',  ( 2.999966428792078865, 227.3061007205240571, 7.376404775963534277 ) ) ;
#7114 = CARTESIAN_POINT ( 'NONE',  ( 4.322356511625540243, 7.650514973136639973, 17.99999999999998934 ) ) ;
#7115 = ORIENTED_EDGE ( 'NONE', *, *, #11087, .F. ) ;
#7116 = ORIENTED_EDGE ( 'NONE', *, *, #6135, .T. ) ;
#7117 = CARTESIAN_POINT ( 'NONE',  ( -2.500000000000000444, 185.8999999978150584, 7.000000000000000000 ) ) ;
#7118 = ORIENTED_EDGE ( 'NONE', *, *, #14093, .T. ) ;
#7119 = ORIENTED_EDGE ( 'NONE', *, *, #8294, .F. ) ;
#7120 = CARTESIAN_POINT ( 'NONE',  ( -5.558508435838179551, -2.857531096718951336, 31.00000000000000000 ) ) ;
#7121 = CARTESIAN_POINT ( 'NONE',  ( -2.817313151351291012, -5.579000502529380512, 24.49999999999999289 ) ) ;
#7122 = CARTESIAN_POINT ( 'NONE',  ( -1.767766952966369542, 185.2999999999999829, 8.767766952966368876 ) ) ;
#7123 = ORIENTED_EDGE ( 'NONE', *, *, #12404, .T. ) ;
#7124 = LINE ( 'NONE', #8403, #11479 ) ;
#7125 = UNCERTAINTY_MEASURE_WITH_UNIT (LENGTH_MEASURE( 1.000000000000000082E-05 ), #9372, 'distance_accuracy_value', 'NONE');
#7126 = DIRECTION ( 'NONE',  ( 0.000000000000000000, -1.000000000000000000, 0.000000000000000000 ) ) ;
#7127 = CARTESIAN_POINT ( 'NONE',  ( -2.849573632035240944, -5.280958870664618665, 12.11561732698604743 ) ) ;
#7128 = CARTESIAN_POINT ( 'NONE',  ( 4.592425496802573972E-16, -2.500000000000000000, -1.199999997815050179 ) ) ;
#7129 = CARTESIAN_POINT ( 'NONE',  ( 2.500000000000000444, 187.8999999978150584, 7.000000000000000000 ) ) ;
#7130 = CARTESIAN_POINT ( 'NONE',  ( -2.817313151351291012, -5.579000502529380512, 24.49999999999999289 ) ) ;
#7131 =( NAMED_UNIT ( * ) SI_UNIT ( $, .STERADIAN. ) SOLID_ANGLE_UNIT ( ) );
#7132 = EDGE_CURVE ( 'NONE', #8233, #721, #2607, .T. ) ;
#7133 = CARTESIAN_POINT ( 'NONE',  ( -1.965116437629976787E-16, 189.6999999978150697, 4.500000000000000000 ) ) ;
#7134 = CARTESIAN_POINT ( 'NONE',  ( 2.856278104602718138, 227.5851434513726019, 8.197675965640897289 ) ) ;
#7135 = CARTESIAN_POINT ( 'NONE',  ( 2.668367453516610421, 5.373994336898141100, 31.13064961348856130 ) ) ;
#7136 = B_SPLINE_CURVE_WITH_KNOTS ( 'NONE', 3,
 ( #12120, #12198, #5850, #8487, #1221, #3447, #11961, #3764, #4736, #12044, #14675, #8564, #13239, #6090, #8642, #2332, #1065, #10775 ),
 .UNSPECIFIED., .F., .F.,
 ( 4, 2, 2, 2, 2, 2, 2, 2, 4 ),
 ( 0.000000000000000000, 0.0003914357524127472687, 0.0007828715048254945375, 0.001174307257238241860, 0.001565743009650989075, 0.001957178762063736290, 0.002348614514476483721, 0.002740050266889230719, 0.003131486019301978150 ),
 .UNSPECIFIED. ) ;
#7137 = CARTESIAN_POINT ( 'NONE',  ( -1.999225930651338912, 189.0000000014894113, 5.488052162623582753 ) ) ;
#7138 = ORIENTED_EDGE ( 'NONE', *, *, #267, .T. ) ;
#7139 = CARTESIAN_POINT ( 'NONE',  ( -3.011385983131360522, 5.190390249166416226, 4.200479458972859348 ) ) ;
#7140 = CARTESIAN_POINT ( 'NONE',  ( 4.286401442266437378, 4.198423832313292081, 17.99999999999998934 ) ) ;
#7142 = VERTEX_POINT ( 'NONE', #7297 ) ;
#7141 = CYLINDRICAL_SURFACE ( 'NONE', #7288, 12.49999999999999822 ) ;
#7143 = CARTESIAN_POINT ( 'NONE',  ( 3.882809187879000756, -4.899079348629999053, 31.97400098023329917 ) ) ;
#7144 = CARTESIAN_POINT ( 'NONE',  ( 2.530388970177701147, 226.7703937237002663, 5.798752065564563907 ) ) ;
#7145 = ORIENTED_EDGE ( 'NONE', *, *, #14457, .F. ) ;
#7146 = CARTESIAN_POINT ( 'NONE',  ( -4.267838854167091078, -4.217593933790421801, 5.262398918055981589 ) ) ;
#7147 = CARTESIAN_POINT ( 'NONE',  ( 2.066987299999999639, 0.8561741729129456191, 1.900000001092474688 ) ) ;
#7148 = CARTESIAN_POINT ( 'NONE',  ( -1.359954704877545772, 226.4297670701539005, 4.794973935041616286 ) ) ;
#7149 = DIRECTION ( 'NONE',  ( -0.000000000000000000, -1.000000000000000000, -0.000000000000000000 ) ) ;
#7150 = CARTESIAN_POINT ( 'NONE',  ( 2.500000000000000000, 187.9300000002185129, 7.000000000000000000 ) ) ;
#7151 = CARTESIAN_POINT ( 'NONE',  ( -0.2624983655900470780, 228.9118722929915748, 8.872930048714067652 ) ) ;
#7152 = CARTESIAN_POINT ( 'NONE',  ( 0.7033144145436343031, 227.6506181221223244, 5.230356066017792571 ) ) ;
#7153 = CARTESIAN_POINT ( 'NONE',  ( 2.500000000000000444, 184.6999999978150697, 7.000000000000000000 ) ) ;
#7154 = CARTESIAN_POINT ( 'NONE',  ( 1.461580736456473018, -1.461580736456472573, 0.1500000010924746052 ) ) ;
#7155 = DIRECTION ( 'NONE',  ( -1.000000000000000000, 0.000000000000000000, 0.000000000000000000 ) ) ;
#7156 = EDGE_LOOP ( 'NONE', ( #13755, #5539, #454, #9821, #10586 ) ) ;
#7158 = CARTESIAN_POINT ( 'NONE',  ( 0.8561741729129455081, 189.1999999989075434, 4.933012699999999029 ) ) ;
#7157 = PRODUCT ( 'BR-012', 'BR-012', '', ( #1457 ) ) ;
#7159 = CIRCLE ( 'NONE', #285, 3.000000000000000888 ) ;
#7160 = CARTESIAN_POINT ( 'NONE',  ( 2.066987300000000527, 186.6499999989075320, 7.000000000000000000 ) ) ;
#7161 = CARTESIAN_POINT ( 'NONE',  ( -3.883588957979214218, -4.898466244118963253, 12.47377282875266324 ) ) ;
#7162 = ORIENTED_EDGE ( 'NONE', *, *, #6612, .T. ) ;
#7163 = LINE ( 'NONE', #11124, #3544 ) ;
#7164 = CARTESIAN_POINT ( 'NONE',  ( 0.7993401192313895898, -6.199366368793636006, 25.11483246936573011 ) ) ;
#7165 = SURFACE_STYLE_USAGE ( .BOTH. , #6214 ) ;
#7166 = CARTESIAN_POINT ( 'NONE',  ( 5.999999999999999112, 185.8606548077538321, 9.048340948986950849 ) ) ;
#7167 = CARTESIAN_POINT ( 'NONE',  ( -6.268043809681822509E-16, 188.0499999989075093, 9.066987300000000971 ) ) ;
#7168 = CARTESIAN_POINT ( 'NONE',  ( 3.421280866381198216, -4.930711975950873516, 29.99995067926688108 ) ) ;
#7169 = CARTESIAN_POINT ( 'NONE',  ( -1.767766952966368432, -1.767766952966369320, 0.3000000021849498211 ) ) ;
#7170 = LINE ( 'NONE', #12008, #6314 ) ;
#7171 = CARTESIAN_POINT ( 'NONE',  ( 5.903347812666358330, -1.076697810262539745, 31.61397738943081492 ) ) ;
#7172 = CARTESIAN_POINT ( 'NONE',  ( 0.1323736289504560126, -6.250000000000000888, 32.00000000000000000 ) ) ;
#7173 = CARTESIAN_POINT ( 'NONE',  ( 5.317509234263995133, 2.779225709350928053, 17.99999999999998934 ) ) ;
#7174 = CARTESIAN_POINT ( 'NONE',  ( -2.897581130414634077E-17, 22.00000000000000000, -8.250000000000003553 ) ) ;
#7175 = ADVANCED_FACE ( 'NONE', ( #4989 ), #10712, .F. ) ;
#7176 = VERTEX_POINT ( 'NONE', #11975 ) ;
#7177 = EDGE_CURVE ( 'NONE', #9802, #7295, #13957, .T. ) ;
#7178 = EDGE_LOOP ( 'NONE', ( #12111, #3834 ) ) ;
#7179 = EDGE_LOOP ( 'NONE', ( #8305, #9306 ) ) ;
#7180 = CARTESIAN_POINT ( 'NONE',  ( -4.286401442266640771, 4.198423832313082471, 11.49999999999998224 ) ) ;
#7181 = EDGE_CURVE ( 'NONE', #10893, #512, #1834, .T. ) ;
#7182 = VERTEX_POINT ( 'NONE', #11892 ) ;
#7183 = PRODUCT_DEFINITION_SHAPE ( 'NONE', 'NONE',  #15761 ) ;
#7184 = CARTESIAN_POINT ( 'NONE',  ( -2.066987299999999639, 0.8561741729129452860, 1.200000001092474733 ) ) ;
#7185 = CARTESIAN_POINT ( 'NONE',  ( -5.770167736194668606, -2.404664418229233824, 12.37367328635990482 ) ) ;
#7186 = DIRECTION ( 'NONE',  ( -0.8660254037844387076, -0.4999999999999998890, 0.000000000000000000 ) ) ;
#7187 = CARTESIAN_POINT ( 'NONE',  ( 2.066987299999999639, 185.9999999989074979, 7.856174172912946396 ) ) ;
#7188 = CARTESIAN_POINT ( 'NONE',  ( -1.035533905932737753, 2.500000000000000444, -1.643000000021849205 ) ) ;
#7189 = CARTESIAN_POINT ( 'NONE',  ( 2.030576276931546336E-13, -6.250000000000000888, 24.49999999999999289 ) ) ;
#7190 = CARTESIAN_POINT ( 'NONE',  ( 1.461580736456473018, -1.461580736456472573, 1.750000001092474999 ) ) ;
#7191 = VECTOR ( 'NONE', #3594, 1000.000000000000000 ) ;
#7192 = DIRECTION ( 'NONE',  ( -1.000000000000000000, 0.000000000000000000, 0.000000000000000000 ) ) ;
#7193 = CARTESIAN_POINT ( 'NONE',  ( 2.900052503084635358, 227.0405808247315917, 6.594625917879634258 ) ) ;
#7194 = CARTESIAN_POINT ( 'NONE',  ( 5.770288754215089355, 2.404361317820048694, 5.873819640450716584 ) ) ;
#7195 = EDGE_LOOP ( 'NONE', ( #2632, #14565, #14968, #10438 ) ) ;
#7196 = ORIENTED_EDGE ( 'NONE', *, *, #7936, .F. ) ;
#7197 = CARTESIAN_POINT ( 'NONE',  ( 2.500000000000000444, 186.2499999978150527, 8.035533905932739529 ) ) ;
#7198 = ORIENTED_EDGE ( 'NONE', *, *, #14464, .F. ) ;
#7199 = ORIENTED_EDGE ( 'NONE', *, *, #2651, .T. ) ;
#7200 = CARTESIAN_POINT ( 'NONE',  ( 0.7988860301922496854, 6.199427171881334075, 30.38455580536195555 ) ) ;
#7201 = CARTESIAN_POINT ( 'NONE',  ( -3.458467055437357995, -5.207305717053783312, 23.52640428276697904 ) ) ;
#7202 = CARTESIAN_POINT ( 'NONE',  ( -3.923477796648640936, -4.541042560386369331, 25.37303779027050510 ) ) ;
#7203 = AXIS2_PLACEMENT_3D ( 'NONE', #6633, #11464, #1601 ) ;
#7204 = CARTESIAN_POINT ( 'NONE',  ( 4.141923667210667404, -4.342011609040446807, 12.11561732698604388 ) ) ;
#7205 = CARTESIAN_POINT ( 'NONE',  ( 5.843318061569083177, -1.367618216965475808, 17.12696220972948069 ) ) ;
#7206 = FACE_OUTER_BOUND ( 'NONE', #14183, .T. ) ;
#7207 = CARTESIAN_POINT ( 'NONE',  ( -1.035533905932738197, -2.500000000000000000, -1.249999997815050223 ) ) ;
#7208 = CARTESIAN_POINT ( 'NONE',  ( 5.317509234263941842, 2.779225709351030638, 30.86760611998364823 ) ) ;
#7209 = FACE_OUTER_BOUND ( 'NONE', #5086, .T. ) ;
#7210 = DIRECTION ( 'NONE',  ( 0.000000000000000000, 0.000000000000000000, -1.000000000000000000 ) ) ;
#7211 = EDGE_CURVE ( 'NONE', #338, #202, #9466, .T. ) ;
#7212 = CARTESIAN_POINT ( 'NONE',  ( 1.767766952966368432, 187.7999999978150356, 8.767766952966368876 ) ) ;
#7213 = B_SPLINE_CURVE_WITH_KNOTS ( 'NONE', 3,
 ( #8190, #4446, #9300, #3244, #8112, #10568, #12074, #15585, #12304, #4687, #1251, #8431, #137, #1172, #3794, #14705, #9855, #6127 ),
 .UNSPECIFIED., .F., .F.,
 ( 4, 2, 2, 2, 2, 2, 2, 2, 4 ),
 ( 0.003131923598876997471, 0.003523316383094313945, 0.003914709167311630419, 0.004306101951528947328, 0.004697494735746264236, 0.005088887519963581144, 0.005480280304180898052, 0.005871673088398214092, 0.006263065872615531000 ),
 .UNSPECIFIED. ) ;
#7214 = CARTESIAN_POINT ( 'NONE',  ( 1.328920255623610380, 226.4243263863947391, 4.778947530392284371 ) ) ;
#7215 = CARTESIAN_POINT ( 'NONE',  ( 4.286401442266517314, 4.198423832313209481, 31.13239388001635888 ) ) ;
#7216 = VECTOR ( 'NONE', #14243, 1000.000000000000000 ) ;
#7217 = CARTESIAN_POINT ( 'NONE',  ( -0.7894119942751186558, 189.4371793396122996, 4.080690743408665000 ) ) ;
#7218 = EDGE_CURVE ( 'NONE', #2429, #13435, #2352, .T. ) ;
#7219 = EDGE_LOOP ( 'NONE', ( #15375, #10689, #4808, #11160 ) ) ;
#7220 = CYLINDRICAL_SURFACE ( 'NONE', #6582, 2.500000000000000000 ) ;
#7221 = DIRECTION ( 'NONE',  ( 0.000000000000000000, 1.000000000000000000, 0.000000000000000000 ) ) ;
#7223 = ORIENTED_EDGE ( 'NONE', *, *, #8957, .F. ) ;
#7222 = CARTESIAN_POINT ( 'NONE',  ( -2.500000000000000888, 187.5999999999999943, 7.000000000000000000 ) ) ;
#7224 = CARTESIAN_POINT ( 'NONE',  ( 0.05965787728184901439, -0.3999999999999923617, 2.543631975746904139 ) ) ;
#7225 = CARTESIAN_POINT ( 'NONE',  ( -2.668367453516831134, 5.373994336898032742, 17.99999999999998934 ) ) ;
#7226 = CARTESIAN_POINT ( 'NONE',  ( 4.290130679986412510, 4.545972905167880995, 23.88439807107078394 ) ) ;
#7227 = CARTESIAN_POINT ( 'NONE',  ( -1.265664690411614835E-16, 2.066987299999999639, 1.250000001092474777 ) ) ;
#7228 = CARTESIAN_POINT ( 'NONE',  ( -0.3835139150651865059, 226.3309889762633134, 4.503752476338783062 ) ) ;
#7229 = CARTESIAN_POINT ( 'NONE',  ( 0.000000000000000000, 184.0000000000000000, 7.000000000000000000 ) ) ;
#7230 = CARTESIAN_POINT ( 'NONE',  ( 1.035533905932737753, 187.2800000002184788, 4.500000000000000888 ) ) ;
#7231 = CARTESIAN_POINT ( 'NONE',  ( 2.500000000000000000, 3.061616997868383141E-16, -0.2999999999999999334 ) ) ;
#7232 = CARTESIAN_POINT ( 'NONE',  ( -1.497718339830098611, 227.8307599607422844, 5.750615970570851943 ) ) ;
#7233 = CARTESIAN_POINT ( 'NONE',  ( 1.939628903789791359, 228.4085481513286311, 7.419301219863100982 ) ) ;
#7234 = CARTESIAN_POINT ( 'NONE',  ( 1.461580736456472573, 1.461580736456472795, 1.950000001092474955 ) ) ;
#7235 = DIRECTION ( 'NONE',  ( 0.8660254037844385966, 0.4999999999999999445, 0.000000000000000000 ) ) ;
#7236 = ORIENTED_EDGE ( 'NONE', *, *, #10283, .F. ) ;
#7237 = CARTESIAN_POINT ( 'NONE',  ( -0.8561741729129457301, 186.8999999989075036, 4.933012699999999029 ) ) ;
#7238 = CARTESIAN_POINT ( 'NONE',  ( 1.461580736456473240, 186.7499999989075263, 5.538419263543526760 ) ) ;
#7239 = CARTESIAN_POINT ( 'NONE',  ( -1.524659305057740610E-16, 189.0000000000000000, 4.500000000000000000 ) ) ;
#7240 = ORIENTED_EDGE ( 'NONE', *, *, #1713, .T. ) ;
#7241 = FACE_OUTER_BOUND ( 'NONE', #15626, .T. ) ;
#7242 = AXIS2_PLACEMENT_3D ( 'NONE', #8556, #14583, #12033 ) ;
#7243 = DIRECTION ( 'NONE',  ( 1.000000000000000000, 0.000000000000000000, 0.000000000000000000 ) ) ;
#7244 = CARTESIAN_POINT ( 'NONE',  ( -3.061616997868383141E-16, 189.0000000000000000, -7.000000000000000000 ) ) ;
#7245 = DIRECTION ( 'NONE',  ( -0.000000000000000000, 1.000000000000000000, -0.000000000000000000 ) ) ;
#7246 = CARTESIAN_POINT ( 'NONE',  ( 1.461580736456473240, 189.1499999989075036, 5.538419263543526760 ) ) ;
#7247 = CARTESIAN_POINT ( 'NONE',  ( 4.195842658231526023, -4.289229542213112367, 30.49560239355786351 ) ) ;
#7248 = CARTESIAN_POINT ( 'NONE',  ( 0.9292488878324430823, 189.7097868069985509, 10.24626543057368799 ) ) ;
#7249 = CARTESIAN_POINT ( 'NONE',  ( -2.500000000000000000, 0.000000000000000000, 0.9000000000000000222 ) ) ;
#7250 = CARTESIAN_POINT ( 'NONE',  ( -2.500000000000000444, 184.4000000000000057, 7.000000000000000000 ) ) ;
#7251 = CARTESIAN_POINT ( 'NONE',  ( 1.035533905932737531, 2.500000000000000444, -2.449999997815050623 ) ) ;
#7252 = CARTESIAN_POINT ( 'NONE',  ( 5.531796221294842830, 2.326749136277297403, 4.126215691297386634 ) ) ;
#7253 = CARTESIAN_POINT ( 'NONE',  ( 1.767766952966369098, 187.2999999999999829, 5.232233047033630235 ) ) ;
#7254 = VECTOR ( 'NONE', #3286, 1000.000000000000114 ) ;
#7255 = ORIENTED_EDGE ( 'NONE', *, *, #8453, .F. ) ;
#7256 = B_SPLINE_CURVE_WITH_KNOTS ( 'NONE', 3,
 ( #549, #2866, #13599, #5419, #8845, #10265, #10033, #11218, #14883, #7640, #12564, #7560, #12485, #15117, #4215, #1585, #6464, #12409 ),
 .UNSPECIFIED., .F., .F.,
 ( 4, 2, 2, 2, 2, 2, 2, 2, 4 ),
 ( 0.003131918686235978661, 0.003523310662250268930, 0.003914702638264559199, 0.004306094614278849035, 0.004697486590293139738, 0.005088878566307429574, 0.005480270542321719410, 0.005871662518336009245, 0.006263054494350299949 ),
 .UNSPECIFIED. ) ;
#7257 = ORIENTED_EDGE ( 'NONE', *, *, #178, .F. ) ;
#7258 = ORIENTED_EDGE ( 'NONE', *, *, #10506, .T. ) ;
#7259 = CARTESIAN_POINT ( 'NONE',  ( 1.499313473695500498, 228.6911157451824579, 8.235372547512890051 ) ) ;
#7260 = ORIENTED_EDGE ( 'NONE', *, *, #11333, .T. ) ;
#7261 = CARTESIAN_POINT ( 'NONE',  ( 0.8561741729129463963, -2.066987299999999195, 1.500000001092474555 ) ) ;
#7262 = PLANE ( 'NONE',  #7810 ) ;
#7263 = CARTESIAN_POINT ( 'NONE',  ( 5.317509234264001350, -2.779225709350912954, 11.49999999999998224 ) ) ;
#7264 = CARTESIAN_POINT ( 'NONE',  ( 1.461580736456472795, 187.7499999989075263, 5.538419263543527649 ) ) ;
#7265 = CARTESIAN_POINT ( 'NONE',  ( 1.035533905932737531, 2.500000000000000444, 1.450000000000000400 ) ) ;
#7266 = EDGE_CURVE ( 'NONE', #5689, #703, #10869, .T. ) ;
#7267 = B_SPLINE_CURVE_WITH_KNOTS ( 'NONE', 3,
 ( #12197, #9670, #13238, #4895, #4974, #13152, #6089, #4653, #5928, #14259, #1295, #2330, #4814, #4735, #8236, #8485, #10693, #107 ),
 .UNSPECIFIED., .F., .F.,
 ( 4, 2, 2, 2, 2, 2, 2, 2, 4 ),
 ( 0.000000000000000000, 0.0003914362731607610437, 0.0007828725463215218706, 0.001174308819482282806, 0.001565745092643043741, 0.001957181365803804460, 0.002348617638964565612, 0.002740053912125326764, 0.003131490185286087483 ),
 .UNSPECIFIED. ) ;
#7268 = CARTESIAN_POINT ( 'NONE',  ( 7.180990026460762010, -3.384707322287334286, 11.49999999999998224 ) ) ;
#7269 = CONTEXT_DEPENDENT_SHAPE_REPRESENTATION ( #7519, #3483 ) ;
#7270 = CARTESIAN_POINT ( 'NONE',  ( 1.461580736456472573, 1.461580736456472795, 1.950000001092474955 ) ) ;
#7271 = CARTESIAN_POINT ( 'NONE',  ( 4.290381260516336503, -4.545736887716150143, 30.38482219624157565 ) ) ;
#7272 = CARTESIAN_POINT ( 'NONE',  ( -1.057007967372188606, 228.1937333886401120, 9.987756413537558942 ) ) ;
#7273 = CARTESIAN_POINT ( 'NONE',  ( 0.000000000000000000, 22.00000000000000000, 0.000000000000000000 ) ) ;
#7274 = ORIENTED_EDGE ( 'NONE', *, *, #7211, .F. ) ;
#7275 = ORIENTED_EDGE ( 'NONE', *, *, #445, .T. ) ;
#7276 = CARTESIAN_POINT ( 'NONE',  ( 1.035533905932738197, 188.5499999978150356, 9.500000000000000000 ) ) ;
#7277 = EDGE_LOOP ( 'NONE', ( #3289, #14486 ) ) ;
#7278 = ORIENTED_EDGE ( 'NONE', *, *, #7284, .T. ) ;
#7279 = CARTESIAN_POINT ( 'NONE',  ( -6.020865209844567190, 1.681180471732243831, 25.47400098023329562 ) ) ;
#7280 = ADVANCED_FACE ( 'NONE', ( #46 ), #9522, .F. ) ;
#7281 = FACE_OUTER_BOUND ( 'NONE', #6322, .T. ) ;
#7282 = CARTESIAN_POINT ( 'NONE',  ( 2.817313151350924638, 5.579000502529565253, 24.49999999999999289 ) ) ;
#7283 = CARTESIAN_POINT ( 'NONE',  ( 4.195795028115062664, -4.289273350251292527, 12.00428920362018737 ) ) ;
#7284 = EDGE_CURVE ( 'NONE', #7295, #9802, #4871, .T. ) ;
#7285 = CARTESIAN_POINT ( 'NONE',  ( -11.25000000000000355, 3.419666426228851687E-14, 2.000000000000001776 ) ) ;
#7286 = CARTESIAN_POINT ( 'NONE',  ( -3.312341048453435910, -5.004306261885476559, 12.47398020122238371 ) ) ;
#7287 = CARTESIAN_POINT ( 'NONE',  ( -2.817313151351230616, -5.579000502529413374, 18.13234125634167171 ) ) ;
#7288 = AXIS2_PLACEMENT_3D ( 'NONE', #8657, #13254, #6189 ) ;
#7289 = CARTESIAN_POINT ( 'NONE',  ( 0.5044069930204643226, -5.979990686694983459, 18.87335743227902896 ) ) ;
#7290 = CARTESIAN_POINT ( 'NONE',  ( 2.500000000000000444, 188.0500000000000114, 5.964466094067262247 ) ) ;
#7291 = DIRECTION ( 'NONE',  ( -1.000000000000000000, 0.000000000000000000, 0.000000000000000000 ) ) ;
#7292 = CARTESIAN_POINT ( 'NONE',  ( 2.500000000000000444, 187.0999999978150754, 7.000000000000000000 ) ) ;
#7293 = CARTESIAN_POINT ( 'NONE',  ( 0.9678947859540896204, 226.3761757439112898, 4.637006245081842337 ) ) ;
#7294 = CARTESIAN_POINT ( 'NONE',  ( 3.312524433819795000, 5.004191858253993708, 31.97408052783100274 ) ) ;
#7295 = VERTEX_POINT ( 'NONE', #10947 ) ;
#7296 = DIRECTION ( 'NONE',  ( 0.000000000000000000, 1.000000000000000000, 0.000000000000000000 ) ) ;
#7297 = CARTESIAN_POINT ( 'NONE',  ( 2.668367453516645504, -5.373994336898123336, 11.49999999999998224 ) ) ;
#7299 = EDGE_LOOP ( 'NONE', ( #8558, #6655, #9731, #13452 ) ) ;
#7298 = CARTESIAN_POINT ( 'NONE',  ( 5.935543223013876712, 0.8771126767605440522, 24.49999999999999289 ) ) ;
#7300 = CARTESIAN_POINT ( 'NONE',  ( 0.000000000000000000, -0.3999999999999941380, 2.450963827680237017 ) ) ;
#7301 = CARTESIAN_POINT ( 'NONE',  ( 7.490007020835748541, -2.433650805992050969, 24.49999999999999289 ) ) ;
#7302 = CARTESIAN_POINT ( 'NONE',  ( 4.069800786343640731, 4.744882212776960984, 23.62618035954928786 ) ) ;
#7303 = CARTESIAN_POINT ( 'NONE',  ( -2.066987299999999639, 0.8561741729129452860, -0.1999999989075250117 ) ) ;
#7304 = CARTESIAN_POINT ( 'NONE',  ( 5.931793676715094499, -0.9035324301688607562, 4.737601081944046832 ) ) ;
#7305 = SURFACE_STYLE_USAGE ( .BOTH. , #9925 ) ;
#7306 = EDGE_CURVE ( 'NONE', #7463, #3603, #6931, .T. ) ;
#7307 = CARTESIAN_POINT ( 'NONE',  ( -5.615811513735013527, 2.743665920700446126, 12.00308643866043745 ) ) ;
#7308 = CARTESIAN_POINT ( 'NONE',  ( 1.035533905932737975, 184.1500000000000341, 4.500000000000000888 ) ) ;
#7309 = CARTESIAN_POINT ( 'NONE',  ( -9.750000000000003553, 3.401296724241641415E-14, 2.000000000000001776 ) ) ;
#7310 = CARTESIAN_POINT ( 'NONE',  ( 1.989829716803914739, 228.2822890550965553, 7.054657748597916722 ) ) ;
#7311 = CARTESIAN_POINT ( 'NONE',  ( 2.066987299999999639, 0.8561741729129456191, 0.3000000010924747662 ) ) ;
#7312 = CARTESIAN_POINT ( 'NONE',  ( 6.176542424588125968, 0.9554180641284963915, 17.99999999999998934 ) ) ;
#7313 = ADVANCED_FACE ( 'NONE', ( #12024 ), #4798, .T. ) ;
#7314 = VERTEX_POINT ( 'NONE', #1358 ) ;
#7315 = CARTESIAN_POINT ( 'NONE',  ( -0.8561741729129472844, 188.7999999989075093, 9.066987300000000971 ) ) ;
#7316 = CARTESIAN_POINT ( 'NONE',  ( 0.8561741729129457301, 185.1999999989075150, 4.933012699999999029 ) ) ;
#7317 = CARTESIAN_POINT ( 'NONE',  ( 6.768587589771821120E-14, -6.250000000000000888, 11.49999999999998224 ) ) ;
#7318 = CARTESIAN_POINT ( 'NONE',  ( 1.237586355860756271, 228.7707919832083689, 8.465482067366952634 ) ) ;
#7319 = VERTEX_POINT ( 'NONE', #7263 ) ;
#7320 = DIRECTION ( 'NONE',  ( 0.000000000000000000, 1.000000000000000000, 0.000000000000000000 ) ) ;
#7321 =( REPRESENTATION_RELATIONSHIP ('NONE','NONE', #11191, #4596 ) REPRESENTATION_RELATIONSHIP_WITH_TRANSFORMATION ( #2644 )SHAPE_REPRESENTATION_RELATIONSHIP( ) );
#7322 = PLANE ( 'NONE',  #12886 ) ;
#7323 = CARTESIAN_POINT ( 'NONE',  ( 0.000000000000000000, 194.5935680195190116, 12.11154058223188201 ) ) ;
#7324 = CARTESIAN_POINT ( 'NONE',  ( -2.513578226966119988, 189.0000000000000568, 6.945885617963185155 ) ) ;
#7325 = CARTESIAN_POINT ( 'NONE',  ( 3.107278289587259934, -5.134157760522006342, 30.12635295315577011 ) ) ;
#7326 = CARTESIAN_POINT ( 'NONE',  ( -1.530808498934191571E-16, 2.500000000000000000, -3.199999997815050623 ) ) ;
#7327 = CARTESIAN_POINT ( 'NONE',  ( -0.2624013748572930349, -5.995472630654521851, 30.02628559691082444 ) ) ;
#7328 = CARTESIAN_POINT ( 'NONE',  ( -1.035533905932737753, 184.2500000000000000, 4.500000000000001776 ) ) ;
#7329 = AXIS2_PLACEMENT_3D ( 'NONE', #10786, #14353, #14685 ) ;
#7330 = CARTESIAN_POINT ( 'NONE',  ( 5.935543223013846514, 0.8771126767607477781, 5.000000000000004441 ) ) ;
#7331 = CARTESIAN_POINT ( 'NONE',  ( 1.767766984964215471, 1.767766920968521616, -2.500000000000000444 ) ) ;
#7332 = VERTEX_POINT ( 'NONE', #1124 ) ;
#7333 = VERTEX_POINT ( 'NONE', #5989 ) ;
#7334 = ORIENTED_EDGE ( 'NONE', *, *, #13611, .F. ) ;
#7335 = CARTESIAN_POINT ( 'NONE',  ( -3.735642931251201393, 4.696778275484337684, 25.47408052783099919 ) ) ;
#7336 = ORIENTED_EDGE ( 'NONE', *, *, #11585, .T. ) ;
#7337 = CIRCLE ( 'NONE', #11893, 7.000000000000000000 ) ;
#7338 = CARTESIAN_POINT ( 'NONE',  ( 1.461580736456473018, -1.461580736456472573, 1.550000001092474822 ) ) ;
#7339 = CARTESIAN_POINT ( 'NONE',  ( -5.615973259022280395, -2.743340227996256875, 12.00389213124966759 ) ) ;
#7340 = CARTESIAN_POINT ( 'NONE',  ( 6.123233995736766282E-16, 6.000000000000000888, 6.000000000000005329 ) ) ;
#7341 = CARTESIAN_POINT ( 'NONE',  ( -1.461580736456473462, 188.1499999989075320, 8.461580736456472351 ) ) ;
#7342 = CARTESIAN_POINT ( 'NONE',  ( 4.592425496802573972E-16, -2.500000000000000000, 1.100000000000000089 ) ) ;
#7343 = FACE_OUTER_BOUND ( 'NONE', #13230, .T. ) ;
#7344 = CARTESIAN_POINT ( 'NONE',  ( -6.142908455506903564, -1.155755562476258325, 25.11517780375841014 ) ) ;
#7345 = CARTESIAN_POINT ( 'NONE',  ( -1.461580736456472351, -1.461580736456473018, -1.849999998907525534 ) ) ;
#7346 = CYLINDRICAL_SURFACE ( 'NONE', #5059, 1.000000000000000888 ) ;
#7347 = CARTESIAN_POINT ( 'NONE',  ( -2.599095426179941271, 226.8075136295145171, 5.908139701444540925 ) ) ;
#7348 = CARTESIAN_POINT ( 'NONE',  ( 6.143020266950966146, 1.155160780047777891, 5.614419472454844851 ) ) ;
#7349 = ORIENTED_EDGE ( 'NONE', *, *, #6124, .T. ) ;
#7350 = B_SPLINE_CURVE_WITH_KNOTS ( 'NONE', 3,
 ( #9312, #15124, #4221, #15439, #14152, #10430, #11456, #2059, #5504, #11766, #1827, #14073, #5583, #15281, #4383, #7883, #6701, #4539 ),
 .UNSPECIFIED., .F., .F.,
 ( 4, 2, 2, 2, 2, 2, 2, 2, 4 ),
 ( 0.003131486019301987691, 0.003522824630466694831, 0.003914163241631402404, 0.004305501852796109544, 0.004696840463960814949, 0.005088179075125522088, 0.005479517686290227493, 0.005870856297454933766, 0.006262194908619640038 ),
 .UNSPECIFIED. ) ;
#7351 = VERTEX_POINT ( 'NONE', #7340 ) ;
#7352 = ORIENTED_EDGE ( 'NONE', *, *, #15177, .F. ) ;
#7353 = ORIENTED_EDGE ( 'NONE', *, *, #13572, .T. ) ;
#7354 = EDGE_CURVE ( 'NONE', #12191, #1121, #12440, .T. ) ;
#7355 = CARTESIAN_POINT ( 'NONE',  ( 2.435767893059086031, 189.0000000000000284, 7.586867366306830007 ) ) ;
#7356 = DIRECTION ( 'NONE',  ( 0.000000000000000000, 0.000000000000000000, 1.000000000000000000 ) ) ;
#7357 = CARTESIAN_POINT ( 'NONE',  ( 3.922396193919052365, -4.541970110199439858, 12.37380682714708691 ) ) ;
#7358 = LINE ( 'NONE', #8715, #13647 ) ;
#7359 = PRESENTATION_LAYER_ASSIGNMENT (  '', '', ( #12427 ) ) ;
#7360 = CARTESIAN_POINT ( 'NONE',  ( -2.692693252389579239, -5.362085866495110764, 11.76382603205595778 ) ) ;
#7361 = CARTESIAN_POINT ( 'NONE',  ( -6.105861027178971945, 1.337741388556887401, 5.799544624688434347 ) ) ;
#7362 = CARTESIAN_POINT ( 'NONE',  ( 1.000049560716691266, -5.916071405810123807, 17.86967799011533131 ) ) ;
#7363 = CARTESIAN_POINT ( 'NONE',  ( 6.250000000000000888, 7.654042494670958593E-16, 53.67766952966368876 ) ) ;
#7364 = DIRECTION ( 'NONE',  ( 0.000000000000000000, -1.000000000000000000, 0.000000000000000000 ) ) ;
#7365 = CARTESIAN_POINT ( 'NONE',  ( -9.825582188149883933E-17, 188.0999999978150754, 4.500000000000000000 ) ) ;
#7366 = CARTESIAN_POINT ( 'NONE',  ( 2.189302528786933877, 227.9503441805575505, 9.272039875547573473 ) ) ;
#7367 = CARTESIAN_POINT ( 'NONE',  ( 5.903347812666351224, 1.076697810262578381, 10.88602261056916198 ) ) ;
#7368 = EDGE_CURVE ( 'NONE', #4232, #2808, #6233, .T. ) ;
#7369 = CARTESIAN_POINT ( 'NONE',  ( -2.110350344527927469, 189.0000000007702852, 8.349190812944474516 ) ) ;
#7370 = EDGE_LOOP ( 'NONE', ( #8307, #2708 ) ) ;
#7371 = EDGE_CURVE ( 'NONE', #12887, #5264, #6245, .T. ) ;
#7372 = CARTESIAN_POINT ( 'NONE',  ( -4.196288036172428626, 4.288789315524856427, 4.496879510976232730 ) ) ;
#7373 = CARTESIAN_POINT ( 'NONE',  ( -0.1306171417087921838, -6.000000000000000888, 10.49999999999998401 ) ) ;
#7374 = CARTESIAN_POINT ( 'NONE',  ( -1.500000000000000222, 0.000000000000000000, -5.500000000000000000 ) ) ;
#7375 = CARTESIAN_POINT ( 'NONE',  ( 2.841163418881454739, -5.567120626447898069, 31.26236973443874945 ) ) ;
#7376 = CARTESIAN_POINT ( 'NONE',  ( -2.817313151351189315, 5.579000502529432026, 5.000000000000004441 ) ) ;
#7377 = CARTESIAN_POINT ( 'NONE',  ( 2.817313151350924638, 5.579000502529565253, 24.49999999999999289 ) ) ;
#7378 = CARTESIAN_POINT ( 'NONE',  ( -1.461580736456472795, 1.461580736456472795, -1.049999998907525045 ) ) ;
#7379 = DIRECTION ( 'NONE',  ( 0.000000000000000000, 1.000000000000000000, 0.000000000000000000 ) ) ;
#7380 = AXIS2_PLACEMENT_3D ( 'NONE', #8001, #12843, #9515 ) ;
#7381 = CARTESIAN_POINT ( 'NONE',  ( -3.061616997868391523E-16, 182.0000000000000000, 9.500000000000000000 ) ) ;
#7382 = CARTESIAN_POINT ( 'NONE',  ( -2.500000000000000444, 184.4000000000000057, 7.000000000000000000 ) ) ;
#7383 = FACE_BOUND ( 'NONE', #3341, .T. ) ;
#7384 = CARTESIAN_POINT ( 'NONE',  ( 1.786693786749917301, 227.9723819745098865, 6.159628423921897244 ) ) ;
#7385 = CARTESIAN_POINT ( 'NONE',  ( 2.066987299999999639, 2.531329380823229670E-16, -0.5499999989075250451 ) ) ;
#7386 = CARTESIAN_POINT ( 'NONE',  ( 2.094888803305876858E-14, -6.250000000000000888, 30.00000000000000000 ) ) ;
#7387 = VERTEX_POINT ( 'NONE', #2395 ) ;
#7388 = CARTESIAN_POINT ( 'NONE',  ( -0.8561741729129458411, 188.4999999989074979, 4.933012699999999029 ) ) ;
#7389 = CARTESIAN_POINT ( 'NONE',  ( -1.461580736456473906, 187.1499999989075320, 8.461580736456474128 ) ) ;
#7390 = DIRECTION ( 'NONE',  ( -0.3090169943749584980, 0.9510565162951498674, 0.000000000000000000 ) ) ;
#7392 = EDGE_LOOP ( 'NONE', ( #6943, #8269 ) ) ;
#7391 = CARTESIAN_POINT ( 'NONE',  ( -1.461580736456473240, 185.7499999989074979, 8.461580736456472351 ) ) ;
#7393 = CARTESIAN_POINT ( 'NONE',  ( -4.143041610105433037, -4.340967609746910760, 23.88602261056917442 ) ) ;
#7394 = CARTESIAN_POINT ( 'NONE',  ( 5.329945432499612501, -2.755769831645169088, 5.262290378359324450 ) ) ;
#7395 = CARTESIAN_POINT ( 'NONE',  ( 5.558508435838239059, -2.857531096718835428, 31.13237410716304510 ) ) ;
#7396 = CARTESIAN_POINT ( 'NONE',  ( 0.9737725088283040176, 6.173885267451808545, 11.23735758726568434 ) ) ;
#7397 = ADVANCED_FACE ( 'NONE', ( #12100 ), #5031, .F. ) ;
#7398 = CARTESIAN_POINT ( 'NONE',  ( -2.504122110289527026, 189.0000000000000568, 7.207938535869628183 ) ) ;
#7399 = CARTESIAN_POINT ( 'NONE',  ( 2.500000000000000444, -1.035533905932737309, 0.4499999999999999556 ) ) ;
#7400 = CARTESIAN_POINT ( 'NONE',  ( 0.000000000000000000, 184.0000000000000000, 7.000000000000000000 ) ) ;
#7401 = CYLINDRICAL_SURFACE ( 'NONE', #6823, 1.500000000000000000 ) ;
#7402 = CARTESIAN_POINT ( 'NONE',  ( 5.783198643800792738, -1.602922020054615038, 10.52622176056705428 ) ) ;
#7403 = CARTESIAN_POINT ( 'NONE',  ( -1.530808498934191571E-16, 2.500000000000000000, -2.399999997815050801 ) ) ;
#7404 = FACE_OUTER_BOUND ( 'NONE', #9010, .T. ) ;
#7405 = EDGE_CURVE ( 'NONE', #15156, #12174, #10478, .T. ) ;
#7406 = AXIS2_PLACEMENT_3D ( 'NONE', #11899, #14128, #770 ) ;
#7407 = CARTESIAN_POINT ( 'NONE',  ( -5.940390500375711369, 6.474944468551510290, 11.49999999999998224 ) ) ;
#7408 = ORIENTED_EDGE ( 'NONE', *, *, #8973, .F. ) ;
#7409 = ORIENTED_EDGE ( 'NONE', *, *, #1043, .T. ) ;
#7410 =( REPRESENTATION_RELATIONSHIP ('NONE','NONE', #11191, #4596 ) REPRESENTATION_RELATIONSHIP_WITH_TRANSFORMATION ( #3517 )SHAPE_REPRESENTATION_RELATIONSHIP( ) );
#7411 = ORIENTED_EDGE ( 'NONE', *, *, #594, .F. ) ;
#7412 = EDGE_CURVE ( 'NONE', #645, #9501, #11491, .T. ) ;
#7413 = FACE_BOUND ( 'NONE', #5513, .T. ) ;
#7414 = EDGE_LOOP ( 'NONE', ( #389, #10133 ) ) ;
#7415 = CARTESIAN_POINT ( 'NONE',  ( 1.461580736456472573, 1.461580736456472795, -0.6499999989075253559 ) ) ;
#7416 = DIRECTION ( 'NONE',  ( -6.123233995736766036E-17, 1.000000000000000000, 0.000000000000000000 ) ) ;
#7417 = DIRECTION ( 'NONE',  ( 0.000000000000000000, -2.775557561562887900E-16, 1.000000000000000000 ) ) ;
#7418 = CARTESIAN_POINT ( 'NONE',  ( -4.946672411965113980E-16, 185.8499999989075206, 9.066987300000000971 ) ) ;
#7419 = CARTESIAN_POINT ( 'NONE',  ( 1.035533905932737531, 2.500000000000000444, 2.250000000000000444 ) ) ;
#7420 = DIRECTION ( 'NONE',  ( -1.000000000000000000, 3.326610055774637112E-18, 1.062480551894331163E-17 ) ) ;
#7421 = CARTESIAN_POINT ( 'NONE',  ( 2.668367453516690357, -5.373994336898101132, 31.00000000000000000 ) ) ;
#7422 = CARTESIAN_POINT ( 'NONE',  ( -2.066987299999999195, -0.8561741729129466183, -2.699999998907525178 ) ) ;
#7423 = CARTESIAN_POINT ( 'NONE',  ( 5.859155363331407962, -2.178872204144911340, 10.52599901976669017 ) ) ;
#7424 = CARTESIAN_POINT ( 'NONE',  ( -2.899241975612990352, 227.5395701600909888, 8.063569561630318461 ) ) ;
#7425 = ORIENTED_EDGE ( 'NONE', *, *, #13965, .T. ) ;
#7426 = ORIENTED_EDGE ( 'NONE', *, *, #2195, .T. ) ;
#7427 = ORIENTED_EDGE ( 'NONE', *, *, #4555, .T. ) ;
#7428 = CARTESIAN_POINT ( 'NONE',  ( -5.769755079862274094, -2.405651898699083802, 10.62694108445697161 ) ) ;
#7429 = CARTESIAN_POINT ( 'NONE',  ( 3.158296126777834889, 5.394094919772085994, 4.201121615766614248 ) ) ;
#7430 = CARTESIAN_POINT ( 'NONE',  ( 0.5030929395820232797, 6.230885867001147105, 4.126003191165495743 ) ) ;
#7431 =( BOUNDED_CURVE ( )  B_SPLINE_CURVE ( 2, ( #1483, #11275, #11352, #5004, #7696, #374, #3948, #12621, #2924, #14784, #5159, #15021, #8985, #9933, #6204, #10013, #4029, #2766, #9857, #10166, #14708, #1642, #4113, #13813, #3871, #8744, #11041, #139, #7774, #3796, #2606, #7464, #12306, #6279, #11119, #8823, #222, #7538, #6362, #7620, #12464, #1566, #765, #13972, #9062, #4193, #15408, #5477, #8093, #3001, #3228, #12699, #5397, #10477, #12931, #12850, #10400, #3078, #14046, #6671, #1718, #8170, #4506, #679, #8010, #7926, #6593, #11663, #13889, #3309, #11504, #4271, #605, #1796, #10320, #15172, #5553, #528, #9137, #2031, #9286, #12770, #9361, #7857, #15251, #1874, #14200, #11428, #6749, #11582, #5630, #10246, #4352, #9210, #3155, #1953, #15332, #6828, #4429, #14122, #6906 ),
 .UNSPECIFIED., .F., .F. ) 
 B_SPLINE_CURVE_WITH_KNOTS ( ( 3, 2, 2, 2, 2, 2, 2, 2, 2, 2, 2, 2, 2, 2, 2, 2, 2, 2, 2, 2, 2, 2, 2, 2, 2, 2, 2, 2, 2, 2, 2, 2, 2, 2, 2, 2, 2, 2, 2, 2, 2, 2, 2, 2, 2, 2, 2, 2, 2, 2, 3 ),
 ( 0.000000000000000000, 0.01785714285714285615, 0.03571428571428571230, 0.05357142857142856845, 0.07142857142857142461, 0.08928571428571428770, 0.1071428571428571369, 0.1250000000000000000, 0.1428571428571428492, 0.1607142857142857262, 0.1785714285714285754, 0.1964285714285714246, 0.2142857142857142738, 0.2321428571428571508, 0.2500000000000000000, 0.2678571428571428492, 0.2857142857142856984, 0.3035714285714285476, 0.3214285714285714524, 0.3392857142857143016, 0.3571428571428571508, 0.3750000000000000000, 0.3928571428571428492, 0.4107142857142856984, 0.4285714285714285476, 0.4464285714285714524, 0.4642857142857143016, 0.4821428571428571508, 0.5000000000000000000, 0.5178571428571429047, 0.5357142857142856984, 0.5535714285714286031, 0.5714285714285713969, 0.5892857142857143016, 0.6071428571428570953, 0.6250000000000000000, 0.6428571428571429047, 0.6607142857142856984, 0.6785714285714286031, 0.6964285714285715079, 0.7142857142857143016, 0.7321428571428570953, 0.7500000000000000000, 0.7678571428571429047, 0.7857142857142856984, 0.8035714285714286031, 0.8214285714285713969, 0.8392857142857143016, 0.8571428571428570953, 0.8750000000000000000, 0.8928571428571429047 ),
 .UNSPECIFIED. ) 
 CURVE ( )  GEOMETRIC_REPRESENTATION_ITEM ( )  RATIONAL_B_SPLINE_CURVE ( ( 1.000000000000000000, 0.9238795325112867385, 1.000000000000000000, 0.9238795325112867385, 1.000000000000000000, 0.9238795325112867385, 1.000000000000000000, 0.9238795325112867385, 1.000000000000000000, 0.9238795325112867385, 1.000000000000000000, 0.9238795325112867385, 1.000000000000000000, 0.9238795325112867385, 1.000000000000000000, 0.9238795325112867385, 1.000000000000000000, 0.9238795325112867385, 1.000000000000000000, 0.9238795325112867385, 1.000000000000000000, 0.9238795325112867385, 1.000000000000000000, 0.9238795325112867385, 1.000000000000000000, 0.9238795325112867385, 1.000000000000000000, 0.9238795325112867385, 1.000000000000000000, 0.9238795325112867385, 1.000000000000000000, 0.9238795325112867385, 1.000000000000000000, 0.9238795325112867385, 1.000000000000000000, 0.9238795325112867385, 1.000000000000000000, 0.9238795325112867385, 1.000000000000000000, 0.9238795325112867385, 1.000000000000000000, 0.9238795325112867385, 1.000000000000000000, 0.9238795325112867385, 1.000000000000000000, 0.9238795325112867385, 1.000000000000000000, 0.9238795325112867385, 1.000000000000000000, 0.9238795325112867385, 1.000000000000000000, 0.9238795325112867385, 1.000000000000000000, 0.9238795325112867385, 1.000000000000000000, 0.9238795325112867385, 1.000000000000000000, 0.9238795325112867385, 1.000000000000000000, 0.9238795325112867385, 1.000000000000000000, 0.9238795325112867385, 1.000000000000000000, 0.9238795325112867385, 1.000000000000000000, 0.9238795325112867385, 1.000000000000000000, 0.9238795325112867385, 1.000000000000000000, 0.9238795325112867385, 1.000000000000000000, 0.9238795325112867385, 1.000000000000000000, 0.9238795325112867385, 1.000000000000000000, 0.9238795325112867385, 1.000000000000000000, 0.9238795325112867385, 1.000000000000000000, 0.9238795325112867385, 1.000000000000000000, 0.9238795325112867385, 1.000000000000000000, 0.9238795325112867385, 1.000000000000000000, 0.9238795325112867385, 1.000000000000000000, 0.9238795325112867385, 1.000000000000000000, 0.9238795325112867385, 1.000000000000000000, 0.9238795325112867385, 1.000000000000000000, 0.9238795325112867385, 1.000000000000000000, 0.9238795325112867385, 1.000000000000000000, 0.9238795325112867385, 1.000000000000000000, 0.9238795325112867385, 1.000000000000000000 ) ) 
 REPRESENTATION_ITEM ( '' )  );
#7432 = CARTESIAN_POINT ( 'NONE',  ( -4.196288036172456160, -4.288789315524827117, 18.50312048902377526 ) ) ;
#7433 = CARTESIAN_POINT ( 'NONE',  ( 3.883716939928997913, -4.898343590941240500, 23.52640428276697904 ) ) ;
#7434 = CARTESIAN_POINT ( 'NONE',  ( 0.000000000000000000, 0.000000000000000000, 5.000000000000004441 ) ) ;
#7435 = VECTOR ( 'NONE', #10120, 1000.000000000000000 ) ;
#7436 = CARTESIAN_POINT ( 'NONE',  ( 0.000000000000000000, 0.000000000000000000, 36.00000000000000711 ) ) ;
#7437 = CARTESIAN_POINT ( 'NONE',  ( -2.500000000000000000, 0.000000000000000000, 2.500000000000000000 ) ) ;
#7438 = LINE ( 'NONE', #8648, #5157 ) ;
#7439 = DIRECTION ( 'NONE',  ( 0.000000000000000000, 1.000000000000000000, 0.000000000000000000 ) ) ;
#7440 = CARTESIAN_POINT ( 'NONE',  ( -2.500000000000000444, 186.6999999978150697, 7.000000000000000000 ) ) ;
#7441 = CARTESIAN_POINT ( 'NONE',  ( 2.255245247391631569, 227.9269692368775395, 9.203290779546277278 ) ) ;
#7442 = CARTESIAN_POINT ( 'NONE',  ( -0.1937970382946692660, 188.9999999996763904, 9.496463395928850915 ) ) ;
#7443 = AXIS2_PLACEMENT_3D ( 'NONE', #4801, #9890, #14661 ) ;
#7444 = VERTEX_POINT ( 'NONE', #10993 ) ;
#7445 = DIRECTION ( 'NONE',  ( 0.000000000000000000, 0.000000000000000000, 1.000000000000000000 ) ) ;
#7446 = CARTESIAN_POINT ( 'NONE',  ( 4.435347140101025154, -4.403429997944519059, 11.49999999999998224 ) ) ;
#7447 = DIRECTION ( 'NONE',  ( 1.000000000000000000, 0.000000000000000000, 0.000000000000000000 ) ) ;
#7448 = CARTESIAN_POINT ( 'NONE',  ( 0.9739805876849939592, 5.920636045238133249, 24.76171386814422348 ) ) ;
#7449 = CARTESIAN_POINT ( 'NONE',  ( 2.085888082922780828, 226.5962934794760031, 5.285790551658203995 ) ) ;
#7450 = DIRECTION ( 'NONE',  ( -0.5877852522924685852, -0.8090169943749507819, 0.000000000000000000 ) ) ;
#7451 = CARTESIAN_POINT ( 'NONE',  ( 0.8561741729129463963, -2.066987299999999195, -2.299999998907525267 ) ) ;
#7452 = FACE_OUTER_BOUND ( 'NONE', #4675, .T. ) ;
#7453 = ADVANCED_FACE ( 'NONE', ( #13531 ), #7104, .T. ) ;
#7454 = CARTESIAN_POINT ( 'NONE',  ( -0.9999171162589461925, -6.169494774098552625, 30.86722320330670044 ) ) ;
#7455 = CARTESIAN_POINT ( 'NONE',  ( -5.082197683525802034E-17, 187.3300000002185186, 4.500000000000000000 ) ) ;
#7456 = CARTESIAN_POINT ( 'NONE',  ( -2.500000000000000000, -1.035533905932739307, -0.6500000000000000222 ) ) ;
#7457 = EDGE_CURVE ( 'NONE', #9142, #642, #1047, .T. ) ;
#7458 = B_SPLINE_CURVE_WITH_KNOTS ( 'NONE', 1,
 ( #4100, #13800 ),
 .UNSPECIFIED., .F., .F.,
 ( 2, 2 ),
 ( 0.000000000000000000, 1.000000000000000000 ),
 .UNSPECIFIED. ) ;
#7459 = CARTESIAN_POINT ( 'NONE',  ( 1.132923824227977772, 228.7961917368426157, 8.538838004569329954 ) ) ;
#7460 = FACE_BOUND ( 'NONE', #12889, .T. ) ;
#7461 = CARTESIAN_POINT ( 'NONE',  ( 6.081590040723090063, 1.446205118472959406, 17.12632671364005077 ) ) ;
#7462 = ADVANCED_FACE ( 'NONE', ( #7569 ), #11673, .F. ) ;
#7463 = VERTEX_POINT ( 'NONE', #8854 ) ;
#7464 = CARTESIAN_POINT ( 'NONE',  ( -2.066987299999999195, -0.8561741729129467293, 0.5000000010924746663 ) ) ;
#7465 = CARTESIAN_POINT ( 'NONE',  ( 1.461580736456473462, 185.9499999989075150, 5.538419263543526760 ) ) ;
#7466 = CARTESIAN_POINT ( 'NONE',  ( -5.317509234263865459, -2.779225709351170526, 17.99999999999998934 ) ) ;
#7468 = ORIENTED_EDGE ( 'NONE', *, *, #5363, .T. ) ;
#7467 = CARTESIAN_POINT ( 'NONE',  ( 0.8561741729129460632, 185.8999999989075320, 9.066987299999999195 ) ) ;
#7469 = AXIS2_PLACEMENT_3D ( 'NONE', #15219, #4402, #3427 ) ;
#7470 = DIRECTION ( 'NONE',  ( 0.9996022823964011428, 0.0003845365441984911130, 0.02819803467534520366 ) ) ;
#7471 = CARTESIAN_POINT ( 'NONE',  ( 6.155912734541144182, -1.081577393120831676, 12.00389213124966936 ) ) ;
#7472 = CARTESIAN_POINT ( 'NONE',  ( 5.984377695197238722, -1.807429553002233513, 32.00004906876532118 ) ) ;
#7473 = CARTESIAN_POINT ( 'NONE',  ( 0.000000000000000000, 185.8606548077538321, 9.048340948986950849 ) ) ;
#7474 = EDGE_CURVE ( 'NONE', #13467, #15176, #13199, .T. ) ;
#7475 = CARTESIAN_POINT ( 'NONE',  ( -0.4796817918372051071, 189.0000000000000000, 9.463196806509678538 ) ) ;
#7476 = CARTESIAN_POINT ( 'NONE',  ( 5.317509234264064411, -2.779225709350791718, 24.63239388001634111 ) ) ;
#7477 = CARTESIAN_POINT ( 'NONE',  ( -1.035533905932738197, -2.500000000000000000, -2.049999997815050268 ) ) ;
#7478 = DIRECTION ( 'NONE',  ( 1.000000000000000000, 0.000000000000000000, 0.000000000000000000 ) ) ;
#7479 = DIRECTION ( 'NONE',  ( -1.062480551894329776E-17, -2.775557561562888393E-16, 1.000000000000000000 ) ) ;
#7480 = CARTESIAN_POINT ( 'NONE',  ( -5.842945980534664407, 1.369128644668877515, 10.62621569129736976 ) ) ;
#7481 = CARTESIAN_POINT ( 'NONE',  ( -5.621278735166202800, -2.101423246382545962, 12.47408052783098853 ) ) ;
#7482 = CARTESIAN_POINT ( 'NONE',  ( 4.005785023174299297, 4.467917056767537254, 23.70047945897283270 ) ) ;
#7483 = EDGE_LOOP ( 'NONE', ( #11725, #15611 ) ) ;
#7484 = CARTESIAN_POINT ( 'NONE',  ( -1.461580736456473018, 187.9499999989075150, 5.538419263543527649 ) ) ;
#7485 = EDGE_LOOP ( 'NONE', ( #15397, #847, #8, #8710 ) ) ;
#7486 = EDGE_LOOP ( 'NONE', ( #14634, #15623 ) ) ;
#7487 = CARTESIAN_POINT ( 'NONE',  ( -5.746837578675942915, -1.729433780394465936, 25.49995053646222232 ) ) ;
#7488 = ORIENTED_EDGE ( 'NONE', *, *, #5139, .T. ) ;
#7489 = CARTESIAN_POINT ( 'NONE',  ( -1.461580736456472795, 1.461580736456472795, -0.4499999989075252338 ) ) ;
#7490 = DIRECTION ( 'NONE',  ( -1.000000000000000000, 0.000000000000000000, 0.000000000000000000 ) ) ;
#7491 = CARTESIAN_POINT ( 'NONE',  ( -1.488442273571260133, 228.1302346159642696, 9.801076297958973171 ) ) ;
#7492 = CARTESIAN_POINT ( 'NONE',  ( 0.000000000000000000, 6.250000000000000888, 25.49999999999999645 ) ) ;
#7493 = CARTESIAN_POINT ( 'NONE',  ( -2.500000000000000444, 1.035533905932737753, 1.649999999999999911 ) ) ;
#7494 = VECTOR ( 'NONE', #1055, 1000.000000000000114 ) ;
#7495 = CARTESIAN_POINT ( 'NONE',  ( 13.50000000000000000, 0.000000000000000000, -2.000000000000000444 ) ) ;
#7496 = CONTEXT_DEPENDENT_SHAPE_REPRESENTATION ( #1819, #9202 ) ;
#7497 = CARTESIAN_POINT ( 'NONE',  ( 3.107278289587211972, 5.134157760522037428, 5.873647046844244102 ) ) ;
#7498 = CARTESIAN_POINT ( 'NONE',  ( -1.461580736456472351, -1.461580736456473018, 0.7500000010924748883 ) ) ;
#7499 = EDGE_CURVE ( 'NONE', #8478, #8762, #14148, .T. ) ;
#7500 = CARTESIAN_POINT ( 'NONE',  ( -6.081464507797644359, 1.446657058464150714, 30.12619944752604084 ) ) ;
#7501 = CARTESIAN_POINT ( 'NONE',  ( -2.733336431741188566, 227.6877042401139022, 8.499448515046434949 ) ) ;
#7502 = APPLICATION_CONTEXT ( 'automotive_design' ) ;
#7503 = ORIENTED_EDGE ( 'NONE', *, *, #2535, .F. ) ;
#7504 = VERTEX_POINT ( 'NONE', #10352 ) ;
#7505 = VERTEX_POINT ( 'NONE', #10561 ) ;
#7506 = CARTESIAN_POINT ( 'NONE',  ( 5.375913338529108465, -2.664979843780403090, 30.49571079637980020 ) ) ;
#7507 = CARTESIAN_POINT ( 'NONE',  ( 4.290130679986563500, 4.545972905167733558, 4.384398071070797265 ) ) ;
#7508 = CLOSED_SHELL ( 'NONE', ( #2010, #7453, #4088, #8191, #15430, #13657, #5128, #13129, #13661, #9712, #8829, #8048, #12730 ) ) ;
#7509 = CARTESIAN_POINT ( 'NONE',  ( -6.105861027178926648, -1.337741388557088129, 17.20045537531157720 ) ) ;
#7510 = CARTESIAN_POINT ( 'NONE',  ( 6.000000000000000888, 7.347880794884120722E-16, 0.000000000000000000 ) ) ;
#7511 = CARTESIAN_POINT ( 'NONE',  ( 0.5031281619708453112, 5.980084330432663187, 10.62602272744524079 ) ) ;
#7512 = CARTESIAN_POINT ( 'NONE',  ( -1.035533905932739751, 187.6499999978150584, 9.500000000000003553 ) ) ;
#7513 = CARTESIAN_POINT ( 'NONE',  ( -6.176542424588119751, 0.9554180641285462405, 5.132341256341692137 ) ) ;
#7514 = CARTESIAN_POINT ( 'NONE',  ( -2.931156713028594929, 5.520271803279157119, 18.50436969680152899 ) ) ;
#7515 = APPLICATION_PROTOCOL_DEFINITION ( 'draft international standard', 'automotive_design', 1998, #15331 ) ;
#7516 = CARTESIAN_POINT ( 'NONE',  ( -5.421010862427522170E-17, 187.3699999975965511, 4.500000000000000000 ) ) ;
#7517 = CARTESIAN_POINT ( 'NONE',  ( -1.946166655054753614, 228.1230067974157691, 6.594641503551242678 ) ) ;
#7518 = CARTESIAN_POINT ( 'NONE',  ( -1.826734563482391938, 226.5243062390148623, 5.073637952221710101 ) ) ;
#7519 =( REPRESENTATION_RELATIONSHIP ('NONE','NONE', #11191, #3059 ) REPRESENTATION_RELATIONSHIP_WITH_TRANSFORMATION ( #8626 )SHAPE_REPRESENTATION_RELATIONSHIP( ) );
#7520 = CARTESIAN_POINT ( 'NONE',  ( -2.461562117910376823, 189.0000000012555859, 7.467094330940653002 ) ) ;
#7521 = EDGE_LOOP ( 'NONE', ( #7196, #10589, #7258, #15684 ) ) ;
#7522 = CARTESIAN_POINT ( 'NONE',  ( -5.317509234263920526, -2.779225709351067053, 31.00000000000000000 ) ) ;
#7523 = CARTESIAN_POINT ( 'NONE',  ( -5.615973259022258190, 2.743340227996296843, 23.99610786875029689 ) ) ;
#7524 = CARTESIAN_POINT ( 'NONE',  ( 0.000000000000000000, 6.250000000000000888, 6.000000000000005329 ) ) ;
#7525 = CARTESIAN_POINT ( 'NONE',  ( 5.984377695197213853, 1.807429553002318556, 29.99995093123466816 ) ) ;
#7526 = CARTESIAN_POINT ( 'NONE',  ( 2.999777127831125600, 227.3703607088935712, 7.565575523838102612 ) ) ;
#7527 = CARTESIAN_POINT ( 'NONE',  ( 4.435347140101010055, 4.403429997944536822, 5.000000000000004441 ) ) ;
#7528 = CARTESIAN_POINT ( 'NONE',  ( 2.066987300000000083, -0.8561741729129449530, -2.199999998907525178 ) ) ;
#7529 = CARTESIAN_POINT ( 'NONE',  ( 5.531757352715596987, -2.326874507723346586, 4.126193172852896218 ) ) ;
#7530 = SHAPE_REPRESENTATION_RELATIONSHIP ( 'NONE' , 'NONE' ,  #8978, #12380 ) ;
#7531 = CARTESIAN_POINT ( 'NONE',  ( 2.500000000000000444, 188.8500000000000227, 5.964466094067262247 ) ) ;
#7532 = CARTESIAN_POINT ( 'NONE',  ( -5.454892180317694184E-16, 185.4000000000000057, 9.500000000000001776 ) ) ;
#7533 = DIRECTION ( 'NONE',  ( -1.000000000000000000, 3.326610055774637112E-18, 1.062480551894331163E-17 ) ) ;
#7534 = CARTESIAN_POINT ( 'NONE',  ( 0.5467140873060455375, 228.8869147685435053, 8.800851294624202126 ) ) ;
#7535 = CARTESIAN_POINT ( 'NONE',  ( 1.461580736456472573, 1.461580736456472795, -1.249999998907525223 ) ) ;
#7536 = CARTESIAN_POINT ( 'NONE',  ( 3.254737477227931830, 5.337033878705248036, 12.37367328635990482 ) ) ;
#7537 = VECTOR ( 'NONE', #5338, 1000.000000000000000 ) ;
#7538 = CARTESIAN_POINT ( 'NONE',  ( 0.8561741729129452860, 2.066987299999999639, 0.2000000010924747329 ) ) ;
#7539 = CARTESIAN_POINT ( 'NONE',  ( 0.8561741729129460632, 188.0999999989074922, 9.066987300000000971 ) ) ;
#7540 = CARTESIAN_POINT ( 'NONE',  ( 5.570760634536868317, -2.834026536768118554, 18.26225281721714566 ) ) ;
#7542 = ORIENTED_EDGE ( 'NONE', *, *, #1535, .T. ) ;
#7541 = CARTESIAN_POINT ( 'NONE',  ( 1.461580736456472351, 186.7499999989075263, 8.461580736456474128 ) ) ;
#7543 = EDGE_CURVE ( 'NONE', #1570, #4950, #13396, .T. ) ;
#7544 = CARTESIAN_POINT ( 'NONE',  ( -2.782713018890674572, -5.315928322779141624, 17.49560239355786706 ) ) ;
#7545 = CARTESIAN_POINT ( 'NONE',  ( 5.649053410273110032, -2.675685104943178239, 12.11517780375842790 ) ) ;
#7546 = CARTESIAN_POINT ( 'NONE',  ( -4.435347140101107755, -4.403429997944438234, 18.13060690723497004 ) ) ;
#7547 = CARTESIAN_POINT ( 'NONE',  ( -5.487348639458908828, 2.428538342494374280, 4.199777826161211536 ) ) ;
#7548 = CARTESIAN_POINT ( 'NONE',  ( -0.8738239080079619470, -6.188820299975602346, 12.00355795710141393 ) ) ;
#7549 = CARTESIAN_POINT ( 'NONE',  ( 5.409274167810742995, -2.597759609440460693, 25.11519382448850379 ) ) ;
#7550 = CARTESIAN_POINT ( 'NONE',  ( 0.7305957235815243589, 189.7049259502624921, 10.30464020416732573 ) ) ;
#7551 = DIRECTION ( 'NONE',  ( -1.000000000000000000, 0.000000000000000000, 0.000000000000000000 ) ) ;
#7552 = CARTESIAN_POINT ( 'NONE',  ( 2.848727059636119385, -5.281416301279810099, 5.614425215719389683 ) ) ;
#7553 = CARTESIAN_POINT ( 'NONE',  ( -4.154121946520940689, 4.670585111242914422, 30.20112161576660981 ) ) ;
#7554 = CARTESIAN_POINT ( 'NONE',  ( -5.375763363753415014, -2.665284979407607668, 12.00389795015984973 ) ) ;
#7555 = CARTESIAN_POINT ( 'NONE',  ( -5.782947755040645177, -1.603807858344059145, 10.52601979877758964 ) ) ;
#7556 = EDGE_LOOP ( 'NONE', ( #13215, #9748, #11604 ) ) ;
#7557 = CARTESIAN_POINT ( 'NONE',  ( -2.066987300000000971, 185.6999999989075434, 7.856174172912944620 ) ) ;
#7558 = AXIS2_PLACEMENT_3D ( 'NONE', #13942, #10298, #6494 ) ;
#7559 = EDGE_LOOP ( 'NONE', ( #3096, #11144, #14253, #3438 ) ) ;
#7560 = CARTESIAN_POINT ( 'NONE',  ( -5.842988226680518871, -1.369004370660901193, 23.62619317285289000 ) ) ;
#7561 = EDGE_CURVE ( 'NONE', #7562, #5302, #2118, .T. ) ;
#7562 = VERTEX_POINT ( 'NONE', #6270 ) ;
#7563 = CARTESIAN_POINT ( 'NONE',  ( -5.931817299736819038, -0.9033986943604223052, 24.76229037835931734 ) ) ;
#7564 = SURFACE_STYLE_FILL_AREA ( #2712 ) ;
#7565 = B_SPLINE_CURVE_WITH_KNOTS ( 'NONE', 3,
 ( #7524, #12370, #10155, #13725, #11261, #361, #5227, #15009, #10074, #14924, #4099, #7680, #15083, #12605, #6579, #11414, #515, #5385 ),
 .UNSPECIFIED., .F., .F.,
 ( 4, 2, 2, 2, 2, 2, 2, 2, 4 ),
 ( 0.000000000000000000, 0.0003914362731607609353, 0.0007828725463215216538, 0.001174308819482282372, 0.001565745092643043091, 0.001957181365803803592, 0.002348617638964564745, 0.002740053912125325897, 0.003131490185286086615 ),
 .UNSPECIFIED. ) ;
#7566 = ORIENTED_EDGE ( 'NONE', *, *, #869, .T. ) ;
#7567 = CARTESIAN_POINT ( 'NONE',  ( -2.066987299999999639, 0.8561741729129452860, -1.999999998907524779 ) ) ;
#7568 = CARTESIAN_POINT ( 'NONE',  ( 0.6156307853269531449, 5.969051238897255196, 5.798705734106810006 ) ) ;
#7569 = FACE_OUTER_BOUND ( 'NONE', #8870, .T. ) ;
#7570 = DIRECTION ( 'NONE',  ( 0.9510565162951500895, 0.3090169943749582204, 0.000000000000000000 ) ) ;
#7571 = CARTESIAN_POINT ( 'NONE',  ( -1.035533905932738197, -2.500000000000000000, 0.2499999999999997780 ) ) ;
#7572 = CIRCLE ( 'NONE', #14945, 12.49999999999999822 ) ;
#7573 = CARTESIAN_POINT ( 'NONE',  ( -3.011139120916495049, -5.190534000030354811, 10.70068193741825624 ) ) ;
#7574 = CARTESIAN_POINT ( 'NONE',  ( 2.668367453516584220, -5.373994336898154422, 17.99999999999998934 ) ) ;
#7575 = CARTESIAN_POINT ( 'NONE',  ( -1.461580736456472351, -1.461580736456473018, -0.8499999989075254225 ) ) ;
#7576 = CARTESIAN_POINT ( 'NONE',  ( 5.726049995854485708, -2.506679546901836364, 10.70045537531157365 ) ) ;
#7577 = CARTESIAN_POINT ( 'NONE',  ( -1.502165409303774624, 228.1258990818537598, 9.788304365642131799 ) ) ;
#7578 = VERTEX_POINT ( 'NONE', #1476 ) ;
#7579 = ORIENTED_EDGE ( 'NONE', *, *, #3072, .T. ) ;
#7580 = ORIENTED_EDGE ( 'NONE', *, *, #877, .T. ) ;
#7581 = CARTESIAN_POINT ( 'NONE',  ( 0.8730424326982343386, 5.936362132114442858, 17.49500690218563292 ) ) ;
#7582 = DIRECTION ( 'NONE',  ( 0.000000000000000000, 1.000000000000000000, 0.000000000000000000 ) ) ;
#7583 = VECTOR ( 'NONE', #4641, 1000.000000000000114 ) ;
#7584 = ORIENTED_EDGE ( 'NONE', *, *, #6785, .T. ) ;
#7585 = CARTESIAN_POINT ( 'NONE',  ( -0.5042987395407722007, -5.979983180450076041, 5.873293041799771963 ) ) ;
#7586 = EDGE_CURVE ( 'NONE', #1426, #12192, #295, .T. ) ;
#7587 = CARTESIAN_POINT ( 'NONE',  ( 0.9735856429313065608, -5.920699391845023030, 31.26285283906726775 ) ) ;
#7588 = CARTESIAN_POINT ( 'NONE',  ( 0.9739805876848602884, 5.920636045238155454, 11.76171386814421105 ) ) ;
#7589 = CARTESIAN_POINT ( 'NONE',  ( 0.4244143561419055910, -0.3999999999999906408, -2.581346380257606654 ) ) ;
#7590 = CARTESIAN_POINT ( 'NONE',  ( 1.767766952966369320, 186.3999999978150584, 5.232233047033630235 ) ) ;
#7591 = CARTESIAN_POINT ( 'NONE',  ( -5.935543223013826086, -0.8771126767608832253, 17.99999999999998934 ) ) ;
#7592 = DIRECTION ( 'NONE',  ( 0.000000000000000000, 0.000000000000000000, -1.000000000000000000 ) ) ;
#7593 = DIRECTION ( 'NONE',  ( -0.1884548733085422700, 0.000000000000000000, -0.9820818503191378612 ) ) ;
#7594 = EDGE_CURVE ( 'NONE', #8395, #15526, #6956, .T. ) ;
#7595 = CARTESIAN_POINT ( 'NONE',  ( 1.767766952966369320, 186.4699999975965454, 5.232233047033630235 ) ) ;
#7596 = CARTESIAN_POINT ( 'NONE',  ( -1.990689658724532629, 228.2709309767465697, 7.021854970500988280 ) ) ;
#7597 = CARTESIAN_POINT ( 'NONE',  ( -2.994031302066835654, 227.3524127508109132, 7.512731884239616242 ) ) ;
#7598 = CARTESIAN_POINT ( 'NONE',  ( -2.686130926226363513, 189.9500051332105670, 5.898299179268767567 ) ) ;
#7599 = EDGE_LOOP ( 'NONE', ( #13365, #3836 ) ) ;
#7600 = DIRECTION ( 'NONE',  ( 0.000000000000000000, 0.000000000000000000, 1.000000000000000000 ) ) ;
#7601 = CARTESIAN_POINT ( 'NONE',  ( 2.897581130414634077E-17, 22.00000000000000000, 9.750000000000003553 ) ) ;
#7602 =( GEOMETRIC_REPRESENTATION_CONTEXT ( 3 ) GLOBAL_UNCERTAINTY_ASSIGNED_CONTEXT ( ( #7125 ) ) GLOBAL_UNIT_ASSIGNED_CONTEXT ( ( #9372, #1011, #4439 ) ) REPRESENTATION_CONTEXT ( 'NONE', 'WORKASPACE' ) );
#7603 = CARTESIAN_POINT ( 'NONE',  ( 6.780834054130108014E-14, -6.250000000000000888, 10.49999999999998224 ) ) ;
#7604 = CARTESIAN_POINT ( 'NONE',  ( 6.105747081304161661, 1.338335777572316587, 30.19973484982324408 ) ) ;
#7605 = CARTESIAN_POINT ( 'NONE',  ( 5.131373506000546314, 7.062729720844130199, 11.49999999999998224 ) ) ;
#7606 = ADVANCED_FACE ( 'NONE', ( #13339 ), #9847, .F. ) ;
#7607 = FACE_BOUND ( 'NONE', #2612, .T. ) ;
#7608 = CARTESIAN_POINT ( 'NONE',  ( -2.066987299999999639, 0.8561741729129452860, -2.599999998907525089 ) ) ;
#7609 = CARTESIAN_POINT ( 'NONE',  ( 5.915755444410804031, -1.003187219519845463, 4.496879510976233618 ) ) ;
#7610 = SHAPE_REPRESENTATION_RELATIONSHIP ( 'NONE' , 'NONE' ,  #3059, #10306 ) ;
#7611 = CARTESIAN_POINT ( 'NONE',  ( -4.152999119457946087, -4.671604476854382959, 30.19973484982325118 ) ) ;
#7612 = B_SPLINE_CURVE_WITH_KNOTS ( 'NONE', 3,
 ( #12136, #2431, #3701, #5863, #1237, #4669, #8578, #13672, #13409, #14355, #8330, #13168, #14921, #3855, #12449, #4988, #10152, #1466 ),
 .UNSPECIFIED., .F., .F.,
 ( 4, 2, 2, 2, 2, 2, 2, 2, 4 ),
 ( 0.003131918686235957410, 0.003523310662250250282, 0.003914702638264542719, 0.004306094614278836025, 0.004697486590293128463, 0.005088878566307420900, 0.005480270542321714206, 0.005871662518336005776, 0.006263054494350299081 ),
 .UNSPECIFIED. ) ;
#7613 = CARTESIAN_POINT ( 'NONE',  ( -1.767766952966369765, 186.9000000000000057, 8.767766952966368876 ) ) ;
#7614 = CYLINDRICAL_SURFACE ( 'NONE', #8062, 5.000000000000000000 ) ;
#7616 = CARTESIAN_POINT ( 'NONE',  ( -1.618809023786734747, 227.8806835185142461, 5.894798052868548410 ) ) ;
#7615 = PRESENTATION_LAYER_ASSIGNMENT (  '', '', ( #3804 ) ) ;
#7617 = CARTESIAN_POINT ( 'NONE',  ( -0.8561741729129458411, -2.066987299999999195, -2.399999998907525356 ) ) ;
#7618 = COLOUR_RGB ( '', 0.31764706, 0.68627451, 0.89019608) ;
#7619 = CARTESIAN_POINT ( 'NONE',  ( 6.176542424588149949, -0.9554180641283412934, 24.49999999999999289 ) ) ;
#7620 = CARTESIAN_POINT ( 'NONE',  ( 2.066987299999999639, 0.8561741729129456191, 0.1000000010924746996 ) ) ;
#7621 = CARTESIAN_POINT ( 'NONE',  ( -1.461580736456473240, 187.7499999989075263, 5.538419263543526760 ) ) ;
#7622 = CARTESIAN_POINT ( 'NONE',  ( -5.408775798201109986, -2.598833957129771388, 18.61397738943081848 ) ) ;
#7624 = ORIENTED_EDGE ( 'NONE', *, *, #8678, .T. ) ;
#7623 = CARTESIAN_POINT ( 'NONE',  ( -1.592421940838084637E-16, 188.6499999989075320, 4.933012699999999029 ) ) ;
#7625 = CARTESIAN_POINT ( 'NONE',  ( -3.458467055437294935, -5.207305717053827721, 17.02640428276697904 ) ) ;
#7626 = ADVANCED_FACE ( 'NONE', ( #214 ), #8814, .F. ) ;
#7627 = AXIS2_PLACEMENT_3D ( 'NONE', #14435, #10940, #1149 ) ;
#7628 = CARTESIAN_POINT ( 'NONE',  ( -1.035533905932739751, 186.8499999978150754, 9.500000000000000000 ) ) ;
#7629 = CARTESIAN_POINT ( 'NONE',  ( -5.999999999999999112, 187.9952603975225429, 3.440894205938198613 ) ) ;
#7630 = CARTESIAN_POINT ( 'NONE',  ( 2.782156709077283629, 5.316215864844116012, 17.49687951097622829 ) ) ;
#7631 = CARTESIAN_POINT ( 'NONE',  ( 2.079732661467729837, 189.0000000025126781, 5.600772965815071558 ) ) ;
#7632 = CARTESIAN_POINT ( 'NONE',  ( -1.767766952966369320, 188.1999999978150697, 5.232233047033630235 ) ) ;
#7633 = CARTESIAN_POINT ( 'NONE',  ( 1.992407597290263954, 189.7567858285134719, 9.623042625840206199 ) ) ;
#7634 = CARTESIAN_POINT ( 'NONE',  ( 5.903472034603569618, -2.056448723544995083, 23.49991780678443121 ) ) ;
#7635 = CARTESIAN_POINT ( 'NONE',  ( 0.000000000000000000, 0.000000000000000000, 0.000000000000000000 ) ) ;
#7636 = CARTESIAN_POINT ( 'NONE',  ( -1.524659305057740610E-16, 189.0000000000000000, 4.500000000000000000 ) ) ;
#7637 = ORIENTED_EDGE ( 'NONE', *, *, #15480, .T. ) ;
#7638 = CARTESIAN_POINT ( 'NONE',  ( -2.066987300000000083, 186.3999999989075320, 6.143825827087054492 ) ) ;
#7639 = EDGE_LOOP ( 'NONE', ( #7353, #2867 ) ) ;
#7640 = CARTESIAN_POINT ( 'NONE',  ( -5.746996058422711329, -1.729015645942137080, 23.49992038825522300 ) ) ;
#7641 = ORIENTED_EDGE ( 'NONE', *, *, #6051, .T. ) ;
#7642 = CARTESIAN_POINT ( 'NONE',  ( 0.000000000000000000, 0.000000000000000000, 2.500000000000000000 ) ) ;
#7643 = VERTEX_POINT ( 'NONE', #3785 ) ;
#7644 = CARTESIAN_POINT ( 'NONE',  ( -1.461580736456472795, 1.461580736456472795, -1.249999998907525223 ) ) ;
#7645 = CARTESIAN_POINT ( 'NONE',  ( 6.123233995736766282E-16, 6.000000000000000888, 6.000000000000005329 ) ) ;
#7646 = CARTESIAN_POINT ( 'NONE',  ( 3.659182332138073087E-16, 190.0875178197511275, 4.201689379953569947 ) ) ;
#7647 = CYLINDRICAL_SURFACE ( 'NONE', #298, 1.000000000000000888 ) ;
#7648 = CARTESIAN_POINT ( 'NONE',  ( -1.035533905932737753, 2.500000000000000444, -1.649999999999999911 ) ) ;
#7649 = CARTESIAN_POINT ( 'NONE',  ( -3.311384659207106118, -5.004923837169439338, 10.52641404563304839 ) ) ;
#7650 = EDGE_CURVE ( 'NONE', #6002, #4153, #53, .T. ) ;
#7651 = CARTESIAN_POINT ( 'NONE',  ( -6.155867707731072613, -1.081837891426109310, 25.00436969680152188 ) ) ;
#7652 = CARTESIAN_POINT ( 'NONE',  ( 2.066987299999999639, 2.531329380823229670E-16, 1.050000001092474822 ) ) ;
#7653 = CARTESIAN_POINT ( 'NONE',  ( 6.021135683317715426, -1.680226122398147615, 10.52622717124729590 ) ) ;
#7654 = CARTESIAN_POINT ( 'NONE',  ( 3.632753594129258801, 4.777047695051034992, 12.49995053646221166 ) ) ;
#7655 = EDGE_CURVE ( 'NONE', #13232, #9629, #14541, .T. ) ;
#7656 = ADVANCED_BREP_SHAPE_REPRESENTATION ( '', ( #15721, #14201 ), #3292 ) ;
#7657 = ORIENTED_EDGE ( 'NONE', *, *, #14425, .F. ) ;
#7658 = ORIENTED_EDGE ( 'NONE', *, *, #6021, .T. ) ;
#7659 = EDGE_LOOP ( 'NONE', ( #13274, #2390, #14418, #5730 ) ) ;
#7660 = DIRECTION ( 'NONE',  ( 0.9510565162951500895, 0.3090169943749582204, 0.000000000000000000 ) ) ;
#7661 = CARTESIAN_POINT ( 'NONE',  ( 13.50000000000000000, -0.001000000000000132727, -2.000000000000000444 ) ) ;
#7662 = EDGE_LOOP ( 'NONE', ( #336, #6910 ) ) ;
#7663 = FACE_OUTER_BOUND ( 'NONE', #2732, .T. ) ;
#7664 = CARTESIAN_POINT ( 'NONE',  ( 0.2619456584322226722, -5.995505046955614148, 30.02607193928647433 ) ) ;
#7665 = CARTESIAN_POINT ( 'NONE',  ( -0.9740856415299394833, 6.173834621338617268, 17.73852653055527995 ) ) ;
#7666 = CARTESIAN_POINT ( 'NONE',  ( 5.558508435838239059, -2.857531096718835428, 31.00000000000000000 ) ) ;
#7667 = CARTESIAN_POINT ( 'NONE',  ( 1.767766952966369320, 184.7999999978150356, 5.232233047033630235 ) ) ;
#7668 = CARTESIAN_POINT ( 'NONE',  ( 2.897581130414634077E-17, 22.00000000000000000, 9.750000000000003553 ) ) ;
#7669 = CARTESIAN_POINT ( 'NONE',  ( -5.725684683139646403, 2.507514573674684222, 5.798878384233398187 ) ) ;
#7670 = CARTESIAN_POINT ( 'NONE',  ( 4.141923667210613225, 4.342011609040499209, 10.88438267301394724 ) ) ;
#7671 = DIRECTION ( 'NONE',  ( 0.000000000000000000, -1.000000000000000000, 0.000000000000000000 ) ) ;
#7672 = AXIS2_PLACEMENT_3D ( 'NONE', #14191, #6738, #14112 ) ;
#7673 = CARTESIAN_POINT ( 'NONE',  ( -2.500000000000000444, 185.1699999975965625, 7.000000000000000000 ) ) ;
#7674 = CARTESIAN_POINT ( 'NONE',  ( -1.498122667687309173, 228.6899413643594983, 8.231980868713440813 ) ) ;
#7675 = CARTESIAN_POINT ( 'NONE',  ( -1.058356156152139738, 226.3870070917984094, 4.668936284651906909 ) ) ;
#7676 = CARTESIAN_POINT ( 'NONE',  ( -1.074555296234348978, 189.7140709984146270, 10.19372410532584894 ) ) ;
#7677 = ORIENTED_EDGE ( 'NONE', *, *, #7740, .F. ) ;
#7678 = CARTESIAN_POINT ( 'NONE',  ( -4.286401442266594586, 4.198423832313132209, 5.130649613488546201 ) ) ;
#7679 = CARTESIAN_POINT ( 'NONE',  ( 2.817313151351126699, -5.579000502529464889, 11.36936067245786397 ) ) ;
#7680 = CARTESIAN_POINT ( 'NONE',  ( -0.8736772044959963957, 6.188841968496059387, 4.496115732928120501 ) ) ;
#7681 = CARTESIAN_POINT ( 'NONE',  ( 5.985119669071111481, 1.805077827356575737, 12.49991741810287138 ) ) ;
#7682 = VECTOR ( 'NONE', #14689, 1000.000000000000000 ) ;
#7683 = CARTESIAN_POINT ( 'NONE',  ( 2.717538370304318551, 226.8807925037416453, 6.123999117906609335 ) ) ;
#7684 = CARTESIAN_POINT ( 'NONE',  ( 3.421280866381043673, -4.930711975950980985, 23.49995067926686687 ) ) ;
#7685 = CARTESIAN_POINT ( 'NONE',  ( -1.767766952966368432, -1.767766952966369320, 1.800000000000000044 ) ) ;
#7686 = LINE ( 'NONE', #6819, #59 ) ;
#7687 =( NAMED_UNIT ( * ) SI_UNIT ( $, .STERADIAN. ) SOLID_ANGLE_UNIT ( ) );
#7688 = CARTESIAN_POINT ( 'NONE',  ( -9.750000000000003553, 22.00000000000000000, -3.401296724241641415E-14 ) ) ;
#7689 = CARTESIAN_POINT ( 'NONE',  ( -1.035533905932737753, 185.0499999999999829, 4.500000000000000888 ) ) ;
#7690 = FACE_BOUND ( 'NONE', #7042, .T. ) ;
#7691 = CARTESIAN_POINT ( 'NONE',  ( 1.161994134746590523, 227.7310455073454136, 5.462634941821782775 ) ) ;
#7692 = DIRECTION ( 'NONE',  ( 0.000000000000000000, 0.000000000000000000, -1.000000000000000000 ) ) ;
#7693 = ADVANCED_FACE ( 'NONE', ( #7452 ), #3709, .F. ) ;
#7694 = AXIS2_PLACEMENT_3D ( 'NONE', #10527, #3129, #15381 ) ;
#7695 = CARTESIAN_POINT ( 'NONE',  ( -4.344502777243535618, -4.493369211529261165, 10.99610786875028623 ) ) ;
#7696 = CARTESIAN_POINT ( 'NONE',  ( -1.265664690411614835E-16, 2.066987299999999639, 1.850000001092474644 ) ) ;
#7697 = CARTESIAN_POINT ( 'NONE',  ( 1.461580736456472573, 188.9499999989075150, 8.461580736456474128 ) ) ;
#7698 = CARTESIAN_POINT ( 'NONE',  ( 6.020822430078836440, -1.681351817312256802, 18.97408542334169823 ) ) ;
#7700 = EDGE_LOOP ( 'NONE', ( #6302, #14988, #4969, #3662, #2790 ) ) ;
#7699 = CARTESIAN_POINT ( 'NONE',  ( 1.461580736456472351, 189.1499999989075320, 8.461580736456474128 ) ) ;
#7701 = CARTESIAN_POINT ( 'NONE',  ( -5.000000000000000000, 0.000000000000000000, 0.000000000000000000 ) ) ;
#7702 = DIRECTION ( 'NONE',  ( 0.5877852522924802425, -0.8090169943749422332, 0.000000000000000000 ) ) ;
#7703 = AXIS2_PLACEMENT_3D ( 'NONE', #15446, #14079, #955 ) ;
#7704 = CARTESIAN_POINT ( 'NONE',  ( -5.999999999999999112, 215.0542865858234336, 7.296348638347391891 ) ) ;
#7705 = CARTESIAN_POINT ( 'NONE',  ( 1.753917781081038241, 189.0000000001399485, 8.787807861841729462 ) ) ;
#7706 = CARTESIAN_POINT ( 'NONE',  ( 0.02899383802118515874, -0.3999999999999941380, -2.522283165497671842 ) ) ;
#7707 = CARTESIAN_POINT ( 'NONE',  ( 5.317509234264000462, -2.779225709350912954, 11.36763921416086554 ) ) ;
#7708 = CARTESIAN_POINT ( 'NONE',  ( -2.782769401326221193, 5.315896561274827015, 30.49571079637980375 ) ) ;
#7709 = FACE_OUTER_BOUND ( 'NONE', #3742, .T. ) ;
#7710 = CARTESIAN_POINT ( 'NONE',  ( 1.530808498934191916E-15, 19.99999999999999645, -12.50000000000000355 ) ) ;
#7711 = ORIENTED_EDGE ( 'NONE', *, *, #13482, .F. ) ;
#7712 = CARTESIAN_POINT ( 'NONE',  ( 2.066987300000000083, 187.6999999989075150, 6.143825827087054492 ) ) ;
#7713 = AXIS2_PLACEMENT_3D ( 'NONE', #2049, #13988, #4369 ) ;
#7714 = EDGE_LOOP ( 'NONE', ( #5179, #14687, #8949, #11294 ) ) ;
#7715 = FACE_BOUND ( 'NONE', #12704, .T. ) ;
#7716 = VERTEX_POINT ( 'NONE', #12221 ) ;
#7717 = DIRECTION ( 'NONE',  ( -0.9510565162951544194, 0.3090169943749447312, 0.000000000000000000 ) ) ;
#7718 = DIRECTION ( 'NONE',  ( -0.3090169943749446202, -0.9510565162951544194, 0.000000000000000000 ) ) ;
#7719 = EDGE_LOOP ( 'NONE', ( #5843, #12718, #432, #5262 ) ) ;
#7720 = CARTESIAN_POINT ( 'NONE',  ( -2.066987299999999639, 0.000000000000000000, -1.149999998907525356 ) ) ;
#7721 = CARTESIAN_POINT ( 'NONE',  ( -0.6152055445544960532, 5.969096820685168225, 18.79904968670266996 ) ) ;
#7722 = CARTESIAN_POINT ( 'NONE',  ( -0.2622538972263849244, 6.245673238944479344, 25.47385994369194862 ) ) ;
#7723 = CARTESIAN_POINT ( 'NONE',  ( 4.592425496802573972E-16, -2.500000000000000000, -2.100000000000000089 ) ) ;
#7724 = CARTESIAN_POINT ( 'NONE',  ( 0.000000000000000000, 184.0000000000000000, 0.000000000000000000 ) ) ;
#7725 = CARTESIAN_POINT ( 'NONE',  ( -4.267838854167249174, 4.217593933790261040, 17.73760108194402108 ) ) ;
#7726 = ITEM_DEFINED_TRANSFORMATION ( 'NONE', 'NONE', #10610,  #14201 ) ;
#7727 = DIRECTION ( 'NONE',  ( 0.9510565162951500895, 0.3090169943749582204, 0.000000000000000000 ) ) ;
#7728 = CARTESIAN_POINT ( 'NONE',  ( -1.265664690411614835E-16, 2.066987299999999639, 0.4500000010924747329 ) ) ;
#7729 = CARTESIAN_POINT ( 'NONE',  ( -0.6139731865239675956, 6.220476368274055368, 30.19975545601933220 ) ) ;
#7730 = VECTOR ( 'NONE', #443, 1000.000000000000000 ) ;
#7731 = EDGE_LOOP ( 'NONE', ( #6387, #12114, #6689, #4887 ) ) ;
#7732 = EDGE_LOOP ( 'NONE', ( #11298, #14966, #13167, #4151 ) ) ;
#7733 =( BOUNDED_SURFACE ( )  B_SPLINE_SURFACE ( 1, 2, ( 
 ( #14097, #8146, #9185, #12906, #654, #8301, #3131, #10374, #10529, #6881, #890, #972, #15224, #11789, #5758, #12824, #6802, #4327, #9334, #3356, #815, #2158, #2007, #15462, #9493, #11714, #5605, #11637, #7984, #15304, #10452, #3205, #15383, #10603, #5526, #1928, #739, #5837, #12980, #4408, #9261, #4564, #9414, #4480, #13139, #14326, #14175, #8225, #3283, #14249, #7031, #11860, #10682, #15543, #4639, #3433, #2239, #175, #13463, #5915, #8388, #1365, #10763, #5039, #12265, #3753, #8628, #6077, #15700, #2565, #1206, #4964, #6239, #4882, #14498, #13303, #12187, #2402, #7345, #14413, #4722, #9892, #6160, #14578, #1052, #8703, #14745, #98, #9658, #10837, #1286, #9740, #11075, #15618, #1129, #7422, #3831, #3675, #9571, #13537, #2646 ),
 ( #12030, #11947, #4802, #8553, #3518, #21, #7270, #10998, #5994, #3595, #7190, #12105, #13226, #13377, #2318, #8471, #2487, #9816, #10921, #14664, #12579, #13924, #6551, #4147, #7652, #5432, #5194, #14978, #256, #3982, #7498, #15132, #5116, #1439, #1598, #13693, #7728, #7808, #6317, #8939, #2881, #3906, #13610, #11154, #407, #10203, #12500, #9020, #8861, #11386, #565, #2803, #12422, #2723, #9970, #6398, #1522, #10048, #14896, #13772, #12344, #14820, #7575, #12659, #4069, #8781, #11231, #1676, #487, #333, #4226, #10278, #6476, #15053, #11310, #5277, #10126, #5358, #13846, #6630, #2959, #1756, #11463, #9095, #4544, #12729, #15208, #8207, #1832, #11843, #3339, #10584, #15445, #12883, #6783, #9394, #8046, #11771, #13043, #11698, #5588 ) ),
 .UNSPECIFIED., .F., .F., .F. ) 
 B_SPLINE_SURFACE_WITH_KNOTS ( ( 2, 2 ),
 ( 3, 2, 2, 2, 2, 2, 2, 2, 2, 2, 2, 2, 2, 2, 2, 2, 2, 2, 2, 2, 2, 2, 2, 2, 2, 2, 2, 2, 2, 2, 2, 2, 2, 2, 2, 2, 2, 2, 2, 2, 2, 2, 2, 2, 2, 2, 2, 2, 2, 2, 3 ),
 ( 0.000000000000000000, 1.000000000000000000 ),
 ( 0.000000000000000000, 0.01785714285714285615, 0.03571428571428571230, 0.05357142857142856845, 0.07142857142857142461, 0.08928571428571428770, 0.1071428571428571369, 0.1250000000000000000, 0.1428571428571428492, 0.1607142857142857262, 0.1785714285714285754, 0.1964285714285714246, 0.2142857142857142738, 0.2321428571428571508, 0.2500000000000000000, 0.2678571428571428492, 0.2857142857142856984, 0.3035714285714285476, 0.3214285714285714524, 0.3392857142857143016, 0.3571428571428571508, 0.3750000000000000000, 0.3928571428571428492, 0.4107142857142856984, 0.4285714285714285476, 0.4464285714285714524, 0.4642857142857143016, 0.4821428571428571508, 0.5000000000000000000, 0.5178571428571429047, 0.5357142857142856984, 0.5535714285714286031, 0.5714285714285713969, 0.5892857142857143016, 0.6071428571428570953, 0.6250000000000000000, 0.6428571428571429047, 0.6607142857142856984, 0.6785714285714286031, 0.6964285714285713969, 0.7142857142857143016, 0.7321428571428570953, 0.7500000000000000000, 0.7678571428571429047, 0.7857142857142856984, 0.8035714285714286031, 0.8214285714285713969, 0.8392857142857143016, 0.8571428571428570953, 0.8750000000000000000, 0.8928571428571429047 ),
 .UNSPECIFIED. ) 
 GEOMETRIC_REPRESENTATION_ITEM ( )  RATIONAL_B_SPLINE_SURFACE ( (
 ( 1.000000000000000000, 0.9238795325112867385, 1.000000000000000000, 0.9238795325112867385, 1.000000000000000000, 0.9238795325112867385, 1.000000000000000000, 0.9238795325112867385, 1.000000000000000000, 0.9238795325112867385, 1.000000000000000000, 0.9238795325112867385, 1.000000000000000000, 0.9238795325112867385, 1.000000000000000000, 0.9238795325112867385, 1.000000000000000000, 0.9238795325112867385, 1.000000000000000000, 0.9238795325112867385, 1.000000000000000000, 0.9238795325112867385, 1.000000000000000000, 0.9238795325112867385, 1.000000000000000000, 0.9238795325112867385, 1.000000000000000000, 0.9238795325112867385, 1.000000000000000000, 0.9238795325112867385, 1.000000000000000000, 0.9238795325112867385, 1.000000000000000000, 0.9238795325112867385, 1.000000000000000000, 0.9238795325112867385, 1.000000000000000000, 0.9238795325112867385, 1.000000000000000000, 0.9238795325112867385, 1.000000000000000000, 0.9238795325112867385, 1.000000000000000000, 0.9238795325112867385, 1.000000000000000000, 0.9238795325112867385, 1.000000000000000000, 0.9238795325112867385, 1.000000000000000000, 0.9238795325112867385, 1.000000000000000000, 0.9238795325112867385, 1.000000000000000000, 0.9238795325112867385, 1.000000000000000000, 0.9238795325112867385, 1.000000000000000000, 0.9238795325112867385, 1.000000000000000000, 0.9238795325112867385, 1.000000000000000000, 0.9238795325112867385, 1.000000000000000000, 0.9238795325112867385, 1.000000000000000000, 0.9238795325112867385, 1.000000000000000000, 0.9238795325112867385, 1.000000000000000000, 0.9238795325112867385, 1.000000000000000000, 0.9238795325112867385, 1.000000000000000000, 0.9238795325112867385, 1.000000000000000000, 0.9238795325112867385, 1.000000000000000000, 0.9238795325112867385, 1.000000000000000000, 0.9238795325112867385, 1.000000000000000000, 0.9238795325112867385, 1.000000000000000000, 0.9238795325112867385, 1.000000000000000000, 0.9238795325112867385, 1.000000000000000000, 0.9238795325112867385, 1.000000000000000000, 0.9238795325112867385, 1.000000000000000000, 0.9238795325112867385, 1.000000000000000000, 0.9238795325112867385, 1.000000000000000000, 0.9238795325112867385, 1.000000000000000000, 0.9238795325112867385, 1.000000000000000000, 0.9238795325112867385, 1.000000000000000000),
 ( 1.000000000000000000, 0.9238795325112867385, 1.000000000000000000, 0.9238795325112867385, 1.000000000000000000, 0.9238795325112867385, 1.000000000000000000, 0.9238795325112867385, 1.000000000000000000, 0.9238795325112867385, 1.000000000000000000, 0.9238795325112867385, 1.000000000000000000, 0.9238795325112867385, 1.000000000000000000, 0.9238795325112867385, 1.000000000000000000, 0.9238795325112867385, 1.000000000000000000, 0.9238795325112867385, 1.000000000000000000, 0.9238795325112867385, 1.000000000000000000, 0.9238795325112867385, 1.000000000000000000, 0.9238795325112867385, 1.000000000000000000, 0.9238795325112867385, 1.000000000000000000, 0.9238795325112867385, 1.000000000000000000, 0.9238795325112867385, 1.000000000000000000, 0.9238795325112867385, 1.000000000000000000, 0.9238795325112867385, 1.000000000000000000, 0.9238795325112867385, 1.000000000000000000, 0.9238795325112867385, 1.000000000000000000, 0.9238795325112867385, 1.000000000000000000, 0.9238795325112867385, 1.000000000000000000, 0.9238795325112867385, 1.000000000000000000, 0.9238795325112867385, 1.000000000000000000, 0.9238795325112867385, 1.000000000000000000, 0.9238795325112867385, 1.000000000000000000, 0.9238795325112867385, 1.000000000000000000, 0.9238795325112867385, 1.000000000000000000, 0.9238795325112867385, 1.000000000000000000, 0.9238795325112867385, 1.000000000000000000, 0.9238795325112867385, 1.000000000000000000, 0.9238795325112867385, 1.000000000000000000, 0.9238795325112867385, 1.000000000000000000, 0.9238795325112867385, 1.000000000000000000, 0.9238795325112867385, 1.000000000000000000, 0.9238795325112867385, 1.000000000000000000, 0.9238795325112867385, 1.000000000000000000, 0.9238795325112867385, 1.000000000000000000, 0.9238795325112867385, 1.000000000000000000, 0.9238795325112867385, 1.000000000000000000, 0.9238795325112867385, 1.000000000000000000, 0.9238795325112867385, 1.000000000000000000, 0.9238795325112867385, 1.000000000000000000, 0.9238795325112867385, 1.000000000000000000, 0.9238795325112867385, 1.000000000000000000, 0.9238795325112867385, 1.000000000000000000, 0.9238795325112867385, 1.000000000000000000, 0.9238795325112867385, 1.000000000000000000, 0.9238795325112867385, 1.000000000000000000, 0.9238795325112867385, 1.000000000000000000) ) ) 
 REPRESENTATION_ITEM ( '' )  SURFACE ( )  );
#7734 = B_SPLINE_CURVE_WITH_KNOTS ( 'NONE', 3,
 ( #6141, #9721, #13208, #2301, #9638, #6059, #9872, #2548, #1187, #4944, #3812, #3733, #2465, #7171, #5018, #4782, #10820, #8449 ),
 .UNSPECIFIED., .F., .F.,
 ( 4, 2, 2, 2, 2, 2, 2, 2, 4 ),
 ( 0.000000000000000000, 0.0003914898357794974410, 0.0007829796715589948820, 0.001174469507338492431, 0.001565959343117989764, 0.001957449178897487096, 0.002348939014676984863, 0.002740428850456482195, 0.003131918686235979528 ),
 .UNSPECIFIED. ) ;
#7735 = EDGE_LOOP ( 'NONE', ( #13126, #13366, #9544, #11335 ) ) ;
#7736 = CARTESIAN_POINT ( 'NONE',  ( -5.558508435838157347, -2.857531096718993080, 11.49999999999998224 ) ) ;
#7737 = CARTESIAN_POINT ( 'NONE',  ( 5.725930890718283983, 2.506952462184149688, 4.200668510924229437 ) ) ;
#7738 = ORIENTED_EDGE ( 'NONE', *, *, #4191, .T. ) ;
#7739 = CARTESIAN_POINT ( 'NONE',  ( -5.570820891630725136, -2.833901239560486562, 17.73763026556123634 ) ) ;
#7740 = EDGE_CURVE ( 'NONE', #7039, #7931, #1319, .T. ) ;
#7741 = CARTESIAN_POINT ( 'NONE',  ( 2.817313151351089839, 5.579000502529481764, 31.00000000000000000 ) ) ;
#7742 = VECTOR ( 'NONE', #15465, 1000.000000000000000 ) ;
#7743 = CARTESIAN_POINT ( 'NONE',  ( -5.409007216690712383, 2.598315788643666302, 5.614425215719389683 ) ) ;
#7744 = CARTESIAN_POINT ( 'NONE',  ( 6.081836621194449677, -1.445163676684796394, 30.12694108445700181 ) ) ;
#7745 = CARTESIAN_POINT ( 'NONE',  ( 9.825582188149883933E-17, 184.8999999978150584, 4.500000000000000000 ) ) ;
#7746 = CARTESIAN_POINT ( 'NONE',  ( -2.500000000000000444, 185.0999999978150754, 7.000000000000000000 ) ) ;
#7747 = CARTESIAN_POINT ( 'NONE',  ( 2.848727059635975056, 5.281416301279890035, 10.88557478428060499 ) ) ;
#7748 = DIRECTION ( 'NONE',  ( 1.000000000000000000, 0.000000000000000000, 1.047444401652940007E-14 ) ) ;
#7749 = CARTESIAN_POINT ( 'NONE',  ( 1.767766952966368432, 187.8699999975965511, 8.767766952966368876 ) ) ;
#7750 = CARTESIAN_POINT ( 'NONE',  ( 1.826454486347603767, 228.0556294925947896, 9.581672574142119814 ) ) ;
#7751 = CARTESIAN_POINT ( 'NONE',  ( -2.961755302830887615, 227.1327330595862861, 6.865988109554851171 ) ) ;
#7752 = EDGE_LOOP ( 'NONE', ( #3192, #14014 ) ) ;
#7753 = ADVANCED_FACE ( 'NONE', ( #4263 ), #1944, .T. ) ;
#7754 = CARTESIAN_POINT ( 'NONE',  ( 2.461020065508804144, 0.5233572909743210433, -2.501033807289417599 ) ) ;
#7755 = ORIENTED_EDGE ( 'NONE', *, *, #2195, .F. ) ;
#7756 = CARTESIAN_POINT ( 'NONE',  ( -1.500000000000000000, 9.750000000000003553, 2.000000000000001776 ) ) ;
#7757 = EDGE_CURVE ( 'NONE', #4447, #5302, #6760, .T. ) ;
#7758 = CARTESIAN_POINT ( 'NONE',  ( -5.940390500375673177, 6.474944468551537824, 31.00000000000000000 ) ) ;
#7759 = CARTESIAN_POINT ( 'NONE',  ( 0.5039005892421982713, -6.230833003620535493, 10.62636388911296415 ) ) ;
#7760 = CARTESIAN_POINT ( 'NONE',  ( 5.935543223013879377, -0.8771126767605279539, 17.99999999999998934 ) ) ;
#7761 = CARTESIAN_POINT ( 'NONE',  ( -9.750000000000003553, 19.99999999999999645, 1.499999999999965583 ) ) ;
#7762 = CARTESIAN_POINT ( 'NONE',  ( 2.668367453516523824, -5.373994336898184621, 24.36935038651144936 ) ) ;
#7763 = AXIS2_PLACEMENT_3D ( 'NONE', #9841, #10870, #14357 ) ;
#7764 = CARTESIAN_POINT ( 'NONE',  ( 2.066987299999999639, 0.8561741729129456191, -2.099999998907525534 ) ) ;
#7765 = DIRECTION ( 'NONE',  ( -1.000000000000000000, 0.000000000000000000, 0.000000000000000000 ) ) ;
#7766 =( NAMED_UNIT ( * ) SI_UNIT ( $, .STERADIAN. ) SOLID_ANGLE_UNIT ( ) );
#7767 = CIRCLE ( 'NONE', #2425, 3.000000000000000000 ) ;
#7768 = DIRECTION ( 'NONE',  ( -0.3090169943749579429, 0.9510565162951502005, 0.000000000000000000 ) ) ;
#7769 = CARTESIAN_POINT ( 'NONE',  ( -2.500000000000000444, 187.5500000000000114, 5.964466094067261359 ) ) ;
#7770 = CARTESIAN_POINT ( 'NONE',  ( -1.497718339830098611, 227.8307599607422844, 5.750615970570851943 ) ) ;
#7771 = CARTESIAN_POINT ( 'NONE',  ( 0.000000000000000000, 0.000000000000000000, -11.50000000000000000 ) ) ;
#7772 = EDGE_CURVE ( 'NONE', #9805, #5611, #7686, .T. ) ;
#7773 = CARTESIAN_POINT ( 'NONE',  ( -2.500000000000000000, -1.035533905932739307, -2.949999997815051067 ) ) ;
#7774 = CARTESIAN_POINT ( 'NONE',  ( 3.796994071234844259E-16, -2.066987299999999639, 0.6500000010924747995 ) ) ;
#7775 = CARTESIAN_POINT ( 'NONE',  ( 1.035533905932737975, 184.9499999999999886, 4.500000000000000888 ) ) ;
#7776 = CARTESIAN_POINT ( 'NONE',  ( -2.849269941562104780, 5.281123252783969768, 18.61519382448850024 ) ) ;
#7778 = ORIENTED_EDGE ( 'NONE', *, *, #14325, .F. ) ;
#7777 = CARTESIAN_POINT ( 'NONE',  ( 0.8561741729129458411, 187.4999999989075263, 9.066987299999999195 ) ) ;
#7779 = CARTESIAN_POINT ( 'NONE',  ( -2.817313151351229727, -5.579000502529412486, 17.86762589283693359 ) ) ;
#7780 = CARTESIAN_POINT ( 'NONE',  ( -2.499999999999998224, 186.7499999978150811, 8.035533905932741305 ) ) ;
#7781 = EDGE_CURVE ( 'NONE', #5458, #3136, #440, .T. ) ;
#7782 = CARTESIAN_POINT ( 'NONE',  ( 3.659182332138577465E-16, 188.6555110544239824, 3.692234042172417574 ) ) ;
#7783 = CARTESIAN_POINT ( 'NONE',  ( 6.176542424588118863, -0.9554180641285446862, 5.000000000000004441 ) ) ;
#7784 = CARTESIAN_POINT ( 'NONE',  ( 1.414552616161247167, 189.0000000003665832, 9.066428890920718686 ) ) ;
#7785 = CYLINDRICAL_SURFACE ( 'NONE', #3248, 0.9999999999999998890 ) ;
#7786 = CARTESIAN_POINT ( 'NONE',  ( -5.666074146198007533, -1.978051345703136121, 6.000049320733126912 ) ) ;
#7787 = CARTESIAN_POINT ( 'NONE',  ( 1.899761157012515467, 190.0238153260214062, 4.888075663000788218 ) ) ;
#7788 = CARTESIAN_POINT ( 'NONE',  ( 5.558508435838322548, -2.857531096718671115, 24.36765874365829987 ) ) ;
#7789 = CARTESIAN_POINT ( 'NONE',  ( -5.408775798201144624, -2.598833957129699002, 12.11397738943082558 ) ) ;
#7790 = CARTESIAN_POINT ( 'NONE',  ( -5.330004929009548142, -2.755647751839476189, 11.23760108194400686 ) ) ;
#7791 = ORIENTED_EDGE ( 'NONE', *, *, #13123, .T. ) ;
#7792 = CARTESIAN_POINT ( 'NONE',  ( 1.461580736456472573, 185.9499999989075150, 8.461580736456474128 ) ) ;
#7793 = ORIENTED_EDGE ( 'NONE', *, *, #14649, .T. ) ;
#7794 = DIRECTION ( 'NONE',  ( 1.000000000000000000, 0.000000000000000000, 0.000000000000000000 ) ) ;
#7795 = ORIENTED_EDGE ( 'NONE', *, *, #10097, .F. ) ;
#7796 = CYLINDRICAL_SURFACE ( 'NONE', #4551, 3.000000000000000888 ) ;
#7797 = APPLICATION_CONTEXT ( 'automotive_design' ) ;
#7798 = ORIENTED_EDGE ( 'NONE', *, *, #5282, .F. ) ;
#7799 = DIRECTION ( 'NONE',  ( 0.000000000000000000, 1.000000000000000000, 0.000000000000000000 ) ) ;
#7800 = CARTESIAN_POINT ( 'NONE',  ( -2.817313151351189315, 5.579000502529432026, 5.000000000000004441 ) ) ;
#7801 = EDGE_CURVE ( 'NONE', #6615, #12950, #7940, .T. ) ;
#7802 = CARTESIAN_POINT ( 'NONE',  ( -0.6139731865237586517, 6.220476368274074019, 23.69975545601929667 ) ) ;
#7803 = CARTESIAN_POINT ( 'NONE',  ( 1.035533905932737531, 2.500000000000000444, 1.550000002184949821 ) ) ;
#7804 = DIRECTION ( 'NONE',  ( 0.1736481776669307753, -0.9848077530122080203, 0.000000000000000000 ) ) ;
#7805 = CARTESIAN_POINT ( 'NONE',  ( -2.782713018890612844, -5.315928322779175375, 10.99560239355786528 ) ) ;
#7806 = CONTEXT_DEPENDENT_SHAPE_REPRESENTATION ( #2642, #8461 ) ;
#7807 = FACE_OUTER_BOUND ( 'NONE', #11760, .T. ) ;
#7808 = CARTESIAN_POINT ( 'NONE',  ( 0.8561741729129451750, 2.066987299999999639, 0.4000000010924749105 ) ) ;
#7809 = CARTESIAN_POINT ( 'NONE',  ( 1.035533905932737975, 186.4499999978150697, 4.500000000000001776 ) ) ;
#7810 = AXIS2_PLACEMENT_3D ( 'NONE', #12336, #10916, #3744 ) ;
#7811 = ORIENTED_EDGE ( 'NONE', *, *, #2500, .F. ) ;
#7812 = VERTEX_POINT ( 'NONE', #15166 ) ;
#7813 = ORIENTED_EDGE ( 'NONE', *, *, #1490, .F. ) ;
#7814 = CARTESIAN_POINT ( 'NONE',  ( 2.996920846510471748, -5.485395142346797925, 18.61441947245482709 ) ) ;
#7815 = CARTESIAN_POINT ( 'NONE',  ( 6.105747081304157220, 1.338335777572337015, 4.199734849823245852 ) ) ;
#7816 = VERTEX_POINT ( 'NONE', #12534 ) ;
#7817 = AXIS2_PLACEMENT_3D ( 'NONE', #4361, #10098, #5406 ) ;
#7818 = CARTESIAN_POINT ( 'NONE',  ( -1.530808498934191571E-16, 2.500000000000000000, 1.600000002184949643 ) ) ;
#7819 =( REPRESENTATION_RELATIONSHIP ('NONE','NONE', #11191, #9569 ) REPRESENTATION_RELATIONSHIP_WITH_TRANSFORMATION ( #12342 )SHAPE_REPRESENTATION_RELATIONSHIP( ) );
#7820 = EDGE_CURVE ( 'NONE', #727, #14255, #8897, .T. ) ;
#7821 = CARTESIAN_POINT ( 'NONE',  ( -2.997451966578434046, 5.485105005465995553, 31.61517780375841369 ) ) ;
#7822 = CARTESIAN_POINT ( 'NONE',  ( 0.8730628416138880299, 6.188929913094940893, 17.49504929893120320 ) ) ;
#7823 = CARTESIAN_POINT ( 'NONE',  ( 1.035533905932738419, 186.1499999978150584, 9.500000000000003553 ) ) ;
#7824 = CARTESIAN_POINT ( 'NONE',  ( 5.866817325727518906, -1.260653813891916997, 12.30022217383879024 ) ) ;
#7825 = CARTESIAN_POINT ( 'NONE',  ( 2.692335458626835543, 5.362264153667240407, 11.23760108194400509 ) ) ;
#7826 = DIRECTION ( 'NONE',  ( 0.000000000000000000, 1.000000000000000000, 0.000000000000000000 ) ) ;
#7827 = CARTESIAN_POINT ( 'NONE',  ( -6.403569081242510563E-16, 186.9699999975965454, 9.500000000000001776 ) ) ;
#7828 = CARTESIAN_POINT ( 'NONE',  ( -0.4531526159469659309, 228.8951261137066524, 8.824566127799945647 ) ) ;
#7829 = CARTESIAN_POINT ( 'NONE',  ( -2.381852405317018029, 227.8773184320497478, 9.057252860304588538 ) ) ;
#7830 = AXIS2_PLACEMENT_3D ( 'NONE', #4930, #8519, #7390 ) ;
#7831 = EDGE_CURVE ( 'NONE', #13744, #15449, #9484, .T. ) ;
#7832 = ORIENTED_EDGE ( 'NONE', *, *, #8351, .T. ) ;
#7833 = VECTOR ( 'NONE', #10530, 1000.000000000000114 ) ;
#7834 = CARTESIAN_POINT ( 'NONE',  ( 1.722248641545789605, -1.834520197013864484, -2.499366215161968885 ) ) ;
#7835 = ORIENTED_EDGE ( 'NONE', *, *, #8923, .F. ) ;
#7836 = CARTESIAN_POINT ( 'NONE',  ( -3.883588957979326128, 4.898466244118876212, 17.02622717124729945 ) ) ;
#7837 = CARTESIAN_POINT ( 'NONE',  ( 2.500000000000000444, 189.5499999978150356, 5.964466094067262247 ) ) ;
#7838 = CARTESIAN_POINT ( 'NONE',  ( -2.849573632035434123, 5.280958870664516525, 23.88438267301393125 ) ) ;
#7839 = CARTESIAN_POINT ( 'NONE',  ( 0.000000000000000000, 0.000000000000000000, 0.000000000000000000 ) ) ;
#7840 = B_SPLINE_CURVE_WITH_KNOTS ( 'NONE', 3,
 ( #10980, #6764, #13904, #15189, #3016, #5491, #6530, #12557, #13669, #7634, #10335, #11518, #9151, #4287, #13986, #3092, #7788, #1656 ),
 .UNSPECIFIED., .F., .F.,
 ( 4, 2, 2, 2, 2, 2, 2, 2, 4 ),
 ( 0.003131486019301993329, 0.003522824630466700035, 0.003914163241631406741, 0.004305501852796113013, 0.004696840463960820153, 0.005088179075125527293, 0.005479517686290233565, 0.005870856297454939837, 0.006262194908619646977 ),
 .UNSPECIFIED. ) ;
#7841 = CARTESIAN_POINT ( 'NONE',  ( 2.767106495899620988, 226.9168529135898780, 6.230221390918345037 ) ) ;
#7842 = CIRCLE ( 'NONE', #3015, 5.000000000000000000 ) ;
#7843 = CARTESIAN_POINT ( 'NONE',  ( 2.668367453516524268, -5.373994336898184621, 24.49999999999999289 ) ) ;
#7844 = STYLED_ITEM ( 'NONE', ( #9423 ), #4889 ) ;
#7845 = CARTESIAN_POINT ( 'NONE',  ( -4.290821322214424249, -4.545321419741505942, 18.61441947245482709 ) ) ;
#7846 = CARTESIAN_POINT ( 'NONE',  ( -1.530808498934191571E-16, 2.500000000000000000, -0.1000000000000002554 ) ) ;
#7847 = CARTESIAN_POINT ( 'NONE',  ( -1.035533905932739751, 188.5499999999999829, 9.500000000000000000 ) ) ;
#7848 = LINE ( 'NONE', #2679, #10034 ) ;
#7849 =( BOUNDED_CURVE ( )  B_SPLINE_CURVE ( 2, ( #8369, #2383, #15602, #4703, #14393, #7328, #14480, #6221, #7250 ),
 .UNSPECIFIED., .F., .F. ) 
 B_SPLINE_CURVE_WITH_KNOTS ( ( 3, 2, 2, 2, 3 ),
 ( 0.000000000000000000, 0.01785714285714285615, 0.03571428571428571230, 0.05357142857142856845, 0.07142857142857142461 ),
 .UNSPECIFIED. ) 
 CURVE ( )  GEOMETRIC_REPRESENTATION_ITEM ( )  RATIONAL_B_SPLINE_CURVE ( ( 1.000000000000000000, 0.9238795325112867385, 1.000000000000000000, 0.9238795325112867385, 1.000000000000000000, 0.9238795325112867385, 1.000000000000000000, 0.9238795325112867385, 1.000000000000000000 ) ) 
 REPRESENTATION_ITEM ( '' )  );
#7850 = CARTESIAN_POINT ( 'NONE',  ( -1.035533905932739529, 184.5499999999999829, 9.500000000000003553 ) ) ;
#7851 = EDGE_CURVE ( 'NONE', #8910, #1133, #5315, .T. ) ;
#7852 = CARTESIAN_POINT ( 'NONE',  ( -1.361823383409473953, 227.7851450847494448, 5.618877607002349173 ) ) ;
#7853 = PRODUCT_DEFINITION_CONTEXT ( 'detailed design', #10449, 'design' ) ;
#7854 = CARTESIAN_POINT ( 'NONE',  ( 5.985119669071152337, -1.805077827356440734, 17.00008258189709309 ) ) ;
#7855 = CARTESIAN_POINT ( 'NONE',  ( -4.291255145204043053, -4.544933371694706459, 10.88603820591927018 ) ) ;
#7856 = EDGE_CURVE ( 'NONE', #9215, #7578, #15289, .T. ) ;
#7857 = CARTESIAN_POINT ( 'NONE',  ( -0.8561741729129455081, 2.066987299999999639, -2.099999998907525089 ) ) ;
#7858 = STYLED_ITEM ( 'NONE', ( #8055 ), #15484 ) ;
#7859 = AXIS2_PLACEMENT_3D ( 'NONE', #4058, #5423, #4218 ) ;
#7860 = CARTESIAN_POINT ( 'NONE',  ( 2.066987299999999639, 188.9999999989074979, 7.856174172912946396 ) ) ;
#7861 = CARTESIAN_POINT ( 'NONE',  ( -3.882673863916437540, 4.899192824800819857, 25.47408542334170178 ) ) ;
#7862 = EDGE_CURVE ( 'NONE', #3215, #786, #15402, .T. ) ;
#7864 = ORIENTED_EDGE ( 'NONE', *, *, #2694, .T. ) ;
#7863 = CARTESIAN_POINT ( 'NONE',  ( -0.8561741729129469514, 188.1999999989075150, 9.066987299999999195 ) ) ;
#7865 = FACE_BOUND ( 'NONE', #9749, .T. ) ;
#7866 = CARTESIAN_POINT ( 'NONE',  ( 3.011899281037277998, 5.190111395030357677, 25.30022217383879379 ) ) ;
#7867 = CARTESIAN_POINT ( 'NONE',  ( 0.2023276174663752591, 0.4000000000000047962, -2.561683098399166081 ) ) ;
#7868 = CARTESIAN_POINT ( 'NONE',  ( 1.705890586619502214, 189.1032960091229143, 9.654523998859355416 ) ) ;
#7869 = DIRECTION ( 'NONE',  ( 0.000000000000000000, 0.000000000000000000, 1.000000000000000000 ) ) ;
#7870 = DIRECTION ( 'NONE',  ( 0.8090169943749510040, -0.5877852522924683631, 0.000000000000000000 ) ) ;
#7871 = CARTESIAN_POINT ( 'NONE',  ( 1.558909820229182230, 228.6656996696739554, 8.161969471806774123 ) ) ;
#7872 = DIRECTION ( 'NONE',  ( -0.9510565162951544194, 0.3090169943749447312, 0.000000000000000000 ) ) ;
#7873 = CARTESIAN_POINT ( 'NONE',  ( 0.01582671320853740182, 0.4000000000000062395, 2.506804715526693261 ) ) ;
#7874 = CARTESIAN_POINT ( 'NONE',  ( 4.195795028114904568, 4.289273350251447070, 23.99571079637980020 ) ) ;
#7875 = EDGE_LOOP ( 'NONE', ( #4556, #12892 ) ) ;
#7876 = CARTESIAN_POINT ( 'NONE',  ( 2.066987300000000971, 184.2999999989074809, 6.143825827087054492 ) ) ;
#7877 = ORIENTED_EDGE ( 'NONE', *, *, #11259, .F. ) ;
#7878 = CARTESIAN_POINT ( 'NONE',  ( 0.000000000000000000, 0.000000000000000000, 36.00000000000000711 ) ) ;
#7879 = EDGE_LOOP ( 'NONE', ( #2980, #9916 ) ) ;
#7880 = DIRECTION ( 'NONE',  ( -6.123233995736766036E-17, 1.000000000000000000, 0.000000000000000000 ) ) ;
#7881 = CARTESIAN_POINT ( 'NONE',  ( -2.849573632035176995, -5.280958870664654192, 5.615617326986058977 ) ) ;
#7882 = CARTESIAN_POINT ( 'NONE',  ( -1.530808498934191571E-16, 2.500000000000000000, -1.700000000000000622 ) ) ;
#7883 = CARTESIAN_POINT ( 'NONE',  ( -2.841519077896070389, -5.566940434250053471, 5.263796168408048537 ) ) ;
#7884 = EDGE_CURVE ( 'NONE', #2649, #3525, #3622, .T. ) ;
#7885 = CARTESIAN_POINT ( 'NONE',  ( -2.500000000000000000, -0.9567085809127248153, 1.846193978810514169 ) ) ;
#7886 = CARTESIAN_POINT ( 'NONE',  ( -5.903843691985222186, -2.055287728870673902, 6.000049068765331839 ) ) ;
#7887 = CARTESIAN_POINT ( 'NONE',  ( -3.011385983131474209, 5.190390249166348724, 17.20047945897284691 ) ) ;
#7888 = CARTESIAN_POINT ( 'NONE',  ( -1.530808498934191571E-16, 2.500000000000000000, -0.7999999978150504898 ) ) ;
#7889 = CARTESIAN_POINT ( 'NONE',  ( 2.840966774240201609, 5.567223638426886723, 31.26190213084010239 ) ) ;
#7890 = CYLINDRICAL_SURFACE ( 'NONE', #3138, 2.500000000000000000 ) ;
#7891 = VERTEX_POINT ( 'NONE', #7048 ) ;
#7892 = EDGE_CURVE ( 'NONE', #920, #12484, #12002, .T. ) ;
#7893 = ORIENTED_EDGE ( 'NONE', *, *, #10036, .T. ) ;
#7894 = EDGE_LOOP ( 'NONE', ( #341, #8374 ) ) ;
#7895 = CARTESIAN_POINT ( 'NONE',  ( 3.566234721238037864, -5.134387337253829564, 18.99991741810287493 ) ) ;
#7896 = CARTESIAN_POINT ( 'NONE',  ( 6.172651332693080306, 0.9815532474594598211, 4.738097869159890507 ) ) ;
#7897 = ORIENTED_EDGE ( 'NONE', *, *, #13872, .F. ) ;
#7898 = CARTESIAN_POINT ( 'NONE',  ( 5.935543223013879377, -0.8771126767605279539, 17.99999999999998934 ) ) ;
#7899 = CARTESIAN_POINT ( 'NONE',  ( -1.035533905932738197, -2.500000000000000000, 0.3500000021849494769 ) ) ;
#7900 = CARTESIAN_POINT ( 'NONE',  ( -5.935543223013862502, 0.8771126767606655106, 5.132360785839114925 ) ) ;
#7901 = CARTESIAN_POINT ( 'NONE',  ( 1.767766952966369098, 188.7999999978150356, 5.232233047033630235 ) ) ;
#7902 = CARTESIAN_POINT ( 'NONE',  ( 2.817313151351004130, -5.579000502529524397, 24.49999999999999289 ) ) ;
#7903 = CARTESIAN_POINT ( 'NONE',  ( 4.005785023174413872, 4.467917056767434225, 10.70047945897283981 ) ) ;
#7904 = ITEM_DEFINED_TRANSFORMATION ( 'NONE', 'NONE', #1271,  #14201 ) ;
#7905 = CARTESIAN_POINT ( 'NONE',  ( -7.894347068410079160E-16, 189.3699999975965511, 9.500000000000001776 ) ) ;
#7906 = CARTESIAN_POINT ( 'NONE',  ( -1.770887355114397321, 228.5581793045761287, 7.851444524843710582 ) ) ;
#7907 = CARTESIAN_POINT ( 'NONE',  ( -1.502165409303774624, 228.1258990818537598, 9.788304365642131799 ) ) ;
#7908 = EDGE_LOOP ( 'NONE', ( #10647, #3911 ) ) ;
#7909 = CARTESIAN_POINT ( 'NONE',  ( 0.5843386044905307664, -2.435052651710797544, -2.500695021345132663 ) ) ;
#7910 = VERTEX_POINT ( 'NONE', #10623 ) ;
#7911 = CARTESIAN_POINT ( 'NONE',  ( -2.931212650151771015, 5.520239928492759240, 17.49574050496989841 ) ) ;
#7912 = FACE_OUTER_BOUND ( 'NONE', #12212, .T. ) ;
#7913 = FACE_OUTER_BOUND ( 'NONE', #6732, .T. ) ;
#7914 = DIRECTION ( 'NONE',  ( 0.000000000000000000, 0.000000000000000000, -1.000000000000000000 ) ) ;
#7915 = CARTESIAN_POINT ( 'NONE',  ( 2.817313151351047207, 5.579000502529503080, 11.49999999999998224 ) ) ;
#7916 = CARTESIAN_POINT ( 'NONE',  ( -0.9999171162587678907, -6.169494774098581935, 24.36722320330673242 ) ) ;
#7917 = AXIS2_PLACEMENT_3D ( 'NONE', #7063, #13995, #7957 ) ;
#7918 = FILL_AREA_STYLE_COLOUR ( '', #8016 ) ;
#7919 = CARTESIAN_POINT ( 'NONE',  ( 1.035533905932739085, -2.500000000000000000, -1.250000000000000222 ) ) ;
#7920 = CARTESIAN_POINT ( 'NONE',  ( 2.668367453516627741, 5.373994336898131330, 4.869383044678627925 ) ) ;
#7921 = CARTESIAN_POINT ( 'NONE',  ( 2.500000000000000444, 1.035533905932737975, 1.450000002184949954 ) ) ;
#7922 = CARTESIAN_POINT ( 'NONE',  ( 1.767766952966369098, 188.0999999999999943, 5.232233047033630235 ) ) ;
#7923 = CARTESIAN_POINT ( 'NONE',  ( -0.8818726034074957365, 227.6760006002180319, 5.303662110480990677 ) ) ;
#7924 = FACE_BOUND ( 'NONE', #4890, .T. ) ;
#7925 = CARTESIAN_POINT ( 'NONE',  ( 6.106056299406752430, -1.336851112280646348, 30.20112161576662047 ) ) ;
#7926 = CARTESIAN_POINT ( 'NONE',  ( -2.066987299999999639, 0.8561741729129455081, -1.199999998907525178 ) ) ;
#7927 = VECTOR ( 'NONE', #10160, 1000.000000000000000 ) ;
#7928 = CARTESIAN_POINT ( 'NONE',  ( -2.500000000000000444, 187.5500000000000114, 5.964466094067261359 ) ) ;
#7929 = CARTESIAN_POINT ( 'NONE',  ( -3.458467055437442372, 5.207305717053728245, 25.47359571723300320 ) ) ;
#7931 = VERTEX_POINT ( 'NONE', #8162 ) ;
#7930 = CARTESIAN_POINT ( 'NONE',  ( -0.2638277032946870215, -5.995407492418050488, 25.47332055281518137 ) ) ;
#7932 = CARTESIAN_POINT ( 'NONE',  ( -8.250000000000003553, 3.401296724241641415E-14, 0.000000000000000000 ) ) ;
#7933 = ADVANCED_FACE ( 'NONE', ( #7209 ), #834, .F. ) ;
#7934 = DIRECTION ( 'NONE',  ( -0.000000000000000000, 1.000000000000000000, -0.000000000000000000 ) ) ;
#7935 =( BOUNDED_CURVE ( )  B_SPLINE_CURVE ( 2, ( #8838, #5174, #11056, #8687, #7403, #7251, #13592 ),
 .UNSPECIFIED., .F., .F. ) 
 B_SPLINE_CURVE_WITH_KNOTS ( ( 3, 2, 2, 3 ),
 ( 0.7142857142857143016, 0.7321428571428570953, 0.7500000000000000000, 0.7678571432794594198 ),
 .UNSPECIFIED. ) 
 CURVE ( )  GEOMETRIC_REPRESENTATION_ITEM ( )  RATIONAL_B_SPLINE_CURVE ( ( 1.000000000000000000, 0.9238795325112867385, 1.000000000000000000, 0.9238795325112867385, 1.000000000000000000, 0.9238795325112867385, 1.000000000000000000 ) ) 
 REPRESENTATION_ITEM ( '' )  );
#7936 = EDGE_CURVE ( 'NONE', #10964, #2943, #579, .T. ) ;
#7937 = CARTESIAN_POINT ( 'NONE',  ( -5.317509234263873452, 2.779225709351156315, 24.49999999999999289 ) ) ;
#7938 = CARTESIAN_POINT ( 'NONE',  ( -2.315215587853216128, 189.7792518546661142, 9.280090613206597894 ) ) ;
#7939 = SURFACE_SIDE_STYLE ('',( #2934 ) ) ;
#7940 = CIRCLE ( 'NONE', #13010, 4.000000000000002665 ) ;
#7941 = CARTESIAN_POINT ( 'NONE',  ( 2.051099020578225574, 189.4035295303465034, 4.809436146376961929 ) ) ;
#7942 = CARTESIAN_POINT ( 'NONE',  ( -2.500000000000000444, 185.0800000002185186, 5.964466094067261359 ) ) ;
#7943 = CARTESIAN_POINT ( 'NONE',  ( -0.9972535833697410146, 227.6950091073211979, 5.358559763169368217 ) ) ;
#7944 = CARTESIAN_POINT ( 'NONE',  ( 1.940097806574041073, 228.1129668193434838, 6.565645474235799917 ) ) ;
#7945 = CARTESIAN_POINT ( 'NONE',  ( 2.817313151351169331, -5.579000502529441796, 31.00000000000000000 ) ) ;
#7946 = DIRECTION ( 'NONE',  ( -6.123233995736766036E-17, 1.000000000000000000, 0.000000000000000000 ) ) ;
#7947 = CARTESIAN_POINT ( 'NONE',  ( -3.311384659207082581, -5.004923837169455325, 30.02641404563305016 ) ) ;
#7948 = EDGE_LOOP ( 'NONE', ( #10767, #10418 ) ) ;
#7949 = CARTESIAN_POINT ( 'NONE',  ( 0.8561741729129451750, 189.3999999989075604, 4.933012699999999029 ) ) ;
#7950 = CARTESIAN_POINT ( 'NONE',  ( -2.817313151351230172, -5.579000502529412486, 17.99999999999998934 ) ) ;
#7951 = ADVANCED_FACE ( 'NONE', ( #2177 ), #13160, .F. ) ;
#7952 = ORIENTED_EDGE ( 'NONE', *, *, #1043, .F. ) ;
#7953 = AXIS2_PLACEMENT_3D ( 'NONE', #12998, #5934, #909 ) ;
#7954 = CARTESIAN_POINT ( 'NONE',  ( -7.490007020835642848, -2.433650805992559896, 24.49999999999999289 ) ) ;
#7955 = DIRECTION ( 'NONE',  ( -1.000000000000000000, 0.000000000000000000, 0.000000000000000000 ) ) ;
#7956 = EDGE_CURVE ( 'NONE', #5801, #8675, #10552, .T. ) ;
#7957 = DIRECTION ( 'NONE',  ( 1.000000000000000000, 0.000000000000000000, 0.000000000000000000 ) ) ;
#7958 = DIRECTION ( 'NONE',  ( -0.3090169943749446202, -0.9510565162951544194, 0.000000000000000000 ) ) ;
#7959 = CARTESIAN_POINT ( 'NONE',  ( 3.780072143464109580, 4.979057943639827677, 16.99991780678442055 ) ) ;
#7960 = CARTESIAN_POINT ( 'NONE',  ( 9.825582188149883933E-17, 184.4499999989075150, 4.933012699999999029 ) ) ;
#7961 = CARTESIAN_POINT ( 'NONE',  ( 2.999999999999999556, -1.732050807568877859, -2.500000000000000000 ) ) ;
#7962 = CARTESIAN_POINT ( 'NONE',  ( 4.592425496802573972E-16, -2.500000000000000000, -1.300000000000000044 ) ) ;
#7963 = CARTESIAN_POINT ( 'NONE',  ( 1.035533905932739085, -2.500000000000000000, -1.250000000000000222 ) ) ;
#7964 = CARTESIAN_POINT ( 'NONE',  ( 3.659182332138577465E-16, 202.3202208672780102, 7.308763624242801349 ) ) ;
#7965 = DIRECTION ( 'NONE',  ( 0.000000000000000000, 1.000000000000000000, 0.000000000000000000 ) ) ;
#7966 = CARTESIAN_POINT ( 'NONE',  ( 4.435347140100995844, 4.403429997944548369, 31.13237410716305575 ) ) ;
#7967 = CARTESIAN_POINT ( 'NONE',  ( 4.005998022989905039, 4.467726698309312461, 12.29931806258173665 ) ) ;
#7968 = VERTEX_POINT ( 'NONE', #11967 ) ;
#7969 = ORIENTED_EDGE ( 'NONE', *, *, #12558, .F. ) ;
#7970 = VERTEX_POINT ( 'NONE', #14194 ) ;
#7971 = CARTESIAN_POINT ( 'NONE',  ( 2.817313151351065859, -5.579000502529494199, 17.99999999999998934 ) ) ;
#7972 = DIRECTION ( 'NONE',  ( -0.000000000000000000, -1.000000000000000000, -0.000000000000000000 ) ) ;
#7973 = VERTEX_POINT ( 'NONE', #5622 ) ;
#7974 = DIRECTION ( 'NONE',  ( -0.000000000000000000, 1.000000000000000000, -0.000000000000000000 ) ) ;
#7975 = VECTOR ( 'NONE', #4848, 1000.000000000000000 ) ;
#7976 = CARTESIAN_POINT ( 'NONE',  ( 2.500000000000000444, -1.035533905932737309, 1.350000002184949421 ) ) ;
#7977 = CARTESIAN_POINT ( 'NONE',  ( 1.734723475976807094E-15, 2.000000000000000000, 15.50000000000000000 ) ) ;
#7978 = CARTESIAN_POINT ( 'NONE',  ( 4.416779112813501662, 4.422345839825947422, 24.76225281721715632 ) ) ;
#7979 = CARTESIAN_POINT ( 'NONE',  ( 1.767766952966368432, 189.3999999978150584, 8.767766952966368876 ) ) ;
#7980 = EDGE_CURVE ( 'NONE', #13830, #6640, #8982, .T. ) ;
#7981 = CARTESIAN_POINT ( 'NONE',  ( 1.035533905932737975, 184.8499999978150754, 4.500000000000001776 ) ) ;
#7982 = FACE_OUTER_BOUND ( 'NONE', #4712, .T. ) ;
#7983 = SHAPE_DEFINITION_REPRESENTATION ( #2582, #8978 ) ;
#7984 = CARTESIAN_POINT ( 'NONE',  ( 3.796994071234844259E-16, -2.066987299999999639, 0.6500000010924747995 ) ) ;
#7985 = CARTESIAN_POINT ( 'NONE',  ( -1.767766952966369765, 189.2699999975965568, 8.767766952966368876 ) ) ;
#7986 = CARTESIAN_POINT ( 'NONE',  ( -1.977913707823687250, 228.3348771801055364, 7.206535253053350409 ) ) ;
#7987 = ADVANCED_FACE ( 'NONE', ( #14434 ), #2023, .F. ) ;
#7988 = CARTESIAN_POINT ( 'NONE',  ( -1.057007967372188606, 228.1937333886401120, 9.987756413537558942 ) ) ;
#7989 = ORIENTED_EDGE ( 'NONE', *, *, #42, .T. ) ;
#7990 = CARTESIAN_POINT ( 'NONE',  ( 4.267936573529295785, -4.217499624512150547, 4.737709621640687097 ) ) ;
#7991 = ORIENTED_EDGE ( 'NONE', *, *, #10365, .T. ) ;
#7992 = CARTESIAN_POINT ( 'NONE',  ( 3.566234721238159544, -5.134387337253744299, 5.999917418102892697 ) ) ;
#7993 = CARTESIAN_POINT ( 'NONE',  ( -7.826584432629735133E-16, 189.2999999978150356, 9.500000000000001776 ) ) ;
#7994 = FACE_OUTER_BOUND ( 'NONE', #10842, .T. ) ;
#7995 = ORIENTED_EDGE ( 'NONE', *, *, #2542, .T. ) ;
#7996 = DIRECTION ( 'NONE',  ( 0.000000000000000000, 0.000000000000000000, 1.000000000000000000 ) ) ;
#7997 = FACE_BOUND ( 'NONE', #5023, .T. ) ;
#7998 =( LENGTH_UNIT ( ) NAMED_UNIT ( * ) SI_UNIT ( .MILLI., .METRE. ) );
#7999 = CARTESIAN_POINT ( 'NONE',  ( -1.035533905932737753, 2.500000000000000444, -1.649999999999999911 ) ) ;
#8000 = DIRECTION ( 'NONE',  ( 0.000000000000000000, -1.000000000000000000, 0.000000000000000000 ) ) ;
#8001 = CARTESIAN_POINT ( 'NONE',  ( 0.000000000000000000, 0.000000000000000000, 0.000000000000000000 ) ) ;
#8002 = DIRECTION ( 'NONE',  ( 0.9510565162951499785, 0.3090169943749582204, 0.000000000000000000 ) ) ;
#8003 = CARTESIAN_POINT ( 'NONE',  ( -6.911788849595090767E-16, 187.7999999999999829, 9.500000000000001776 ) ) ;
#8004 = CIRCLE ( 'NONE', #12313, 1.499999999999999556 ) ;
#8005 = CARTESIAN_POINT ( 'NONE',  ( -0.2609190394019921810, 228.9066108255455276, 8.857734630635405892 ) ) ;
#8006 = UNCERTAINTY_MEASURE_WITH_UNIT (LENGTH_MEASURE( 1.000000000000000082E-05 ), #8244, 'distance_accuracy_value', 'NONE');
#8007 = CARTESIAN_POINT ( 'NONE',  ( 5.935543223013858949, -0.8771126767606638452, 5.000000000000004441 ) ) ;
#8008 = CARTESIAN_POINT ( 'NONE',  ( -5.842988226680554398, 1.369004370660755532, 18.87380682714709579 ) ) ;
#8009 = APPLICATION_CONTEXT ( 'automotive_design' ) ;
#8010 = CARTESIAN_POINT ( 'NONE',  ( -2.066987299999999639, 0.000000000000000000, -1.149999998907525356 ) ) ;
#8011 = CARTESIAN_POINT ( 'NONE',  ( 1.035533905932737753, 187.3499999999999659, 4.500000000000000888 ) ) ;
#8012 = CARTESIAN_POINT ( 'NONE',  ( 4.344265632482025907, -4.493596842505014344, 25.00425949503011225 ) ) ;
#8014 = VERTEX_POINT ( 'NONE', #3376 ) ;
#8013 = CARTESIAN_POINT ( 'NONE',  ( -1.035533905932737753, 2.500000000000000444, -1.549999997815050268 ) ) ;
#8015 = CARTESIAN_POINT ( 'NONE',  ( 9.750000000000003553, 184.0000000000000000, 1.500000000000101696 ) ) ;
#8016 = COLOUR_RGB ( '', 0.72549020, 0.75294118, 0.79215686) ;
#8017 = B_SPLINE_CURVE_WITH_KNOTS ( 'NONE', 3,
 ( #8874, #10137, #2574, #418, #13704, #2734, #14674, #3763, #14830, #3915, #12275, #6249, #13621, #11084, #7585, #8950, #11240, #185 ),
 .UNSPECIFIED., .F., .F.,
 ( 4, 2, 2, 2, 2, 2, 2, 2, 4 ),
 ( 0.003131923598876996603, 0.003523316383094313511, 0.003914709167311630419, 0.004306101951528947328, 0.004697494735746264236, 0.005088887519963581144, 0.005480280304180897184, 0.005871673088398214092, 0.006263065872615531000 ),
 .UNSPECIFIED. ) ;
#8018 = CARTESIAN_POINT ( 'NONE',  ( -5.666074146197961348, 1.978051345703259578, 23.49995067926686687 ) ) ;
#8019 = CARTESIAN_POINT ( 'NONE',  ( -1.933502023194013875, 228.0279153893430077, 9.500182718874965460 ) ) ;
#8020 =( NAMED_UNIT ( * ) PLANE_ANGLE_UNIT ( ) SI_UNIT ( $, .RADIAN. ) );
#8021 = CARTESIAN_POINT ( 'NONE',  ( 2.500000000000000444, -1.035533905932737309, -0.2499999978150503066 ) ) ;
#8022 = CARTESIAN_POINT ( 'NONE',  ( -2.500000000000000444, 185.1300000002185016, 7.000000000000000000 ) ) ;
#8023 = CARTESIAN_POINT ( 'NONE',  ( -1.316422468852913585, 227.7699220668886539, 5.574912663155255466 ) ) ;
#8024 = CARTESIAN_POINT ( 'NONE',  ( 0.8212144138252523984, 228.8542370555972809, 8.706476195820313180 ) ) ;
#8025 = CARTESIAN_POINT ( 'NONE',  ( 5.649053410273064735, 2.675685104943274606, 10.88482219624156322 ) ) ;
#8026 = CARTESIAN_POINT ( 'NONE',  ( 0.0002101186055506396033, 0.4000000000000080158, 2.464086358652667563 ) ) ;
#8027 = DIRECTION ( 'NONE',  ( 0.000000000000000000, 0.000000000000000000, -1.000000000000000000 ) ) ;
#8028 = EDGE_LOOP ( 'NONE', ( #824, #12429, #161, #3759 ) ) ;
#8029 = CARTESIAN_POINT ( 'NONE',  ( -2.066987300000001415, 184.6999999989075150, 7.856174172912944620 ) ) ;
#8030 = EDGE_CURVE ( 'NONE', #14335, #2248, #15095, .T. ) ;
#8031 = CARTESIAN_POINT ( 'NONE',  ( 5.558508435838253270, 2.857531096718811892, 17.99999999999998934 ) ) ;
#8032 = EDGE_LOOP ( 'NONE', ( #14749, #13064, #13836, #490 ) ) ;
#8033 = ADVANCED_FACE ( 'NONE', ( #10856 ), #14681, .F. ) ;
#8034 =( BOUNDED_CURVE ( )  B_SPLINE_CURVE ( 2, ( #11640, #2011, #14252, #14178, #743, #2161, #5608, #3360, #6884 ),
 .UNSPECIFIED., .F., .F. ) 
 B_SPLINE_CURVE_WITH_KNOTS ( ( 3, 2, 2, 2, 3 ),
 ( 0.1428571428571428492, 0.1607142857142857262, 0.1785714285714285754, 0.1964285714285714246, 0.2142857142857142738 ),
 .UNSPECIFIED. ) 
 CURVE ( )  GEOMETRIC_REPRESENTATION_ITEM ( )  RATIONAL_B_SPLINE_CURVE ( ( 1.000000000000000000, 0.9238795325112867385, 1.000000000000000000, 0.9238795325112867385, 1.000000000000000000, 0.9238795325112867385, 1.000000000000000000, 0.9238795325112867385, 1.000000000000000000 ) ) 
 REPRESENTATION_ITEM ( '' )  );
#8035 = DIRECTION ( 'NONE',  ( 0.8090169943749421222, 0.5877852522924802425, 0.000000000000000000 ) ) ;
#8036 = B_SPLINE_CURVE_WITH_KNOTS ( 'NONE', 3,
 ( #3905, #8780, #13609, #7651, #7344, #8860, #12499, #1597, #9739, #8552, #13376, #12186, #1285, #1675, #2958, #1988, #14077, #10277 ),
 .UNSPECIFIED., .F., .F.,
 ( 4, 2, 2, 2, 2, 2, 2, 2, 4 ),
 ( 0.000000000000000000, 0.0003914357524127481361, 0.0007828715048254962722, 0.001174307257238244463, 0.001565743009650992544, 0.001957178762063741927, 0.002348614514476491527, 0.002740050266889241127, 0.003131486019301990727 ),
 .UNSPECIFIED. ) ;
#8037 = CARTESIAN_POINT ( 'NONE',  ( -3.923477796648489058, -4.541042560386503446, 5.873037790270514868 ) ) ;
#8038 = CARTESIAN_POINT ( 'NONE',  ( -1.530808498934191571E-16, 2.500000000000000000, 2.184949703804006660E-09 ) ) ;
#8039 = CARTESIAN_POINT ( 'NONE',  ( 0.000000000000000000, 0.4000000000000062395, 2.749999999999994227 ) ) ;
#8040 = CYLINDRICAL_SURFACE ( 'NONE', #3039, 1.500000000000000000 ) ;
#8041 = CARTESIAN_POINT ( 'NONE',  ( 5.409423237179108668, -2.597448116730828982, 23.88438267301394191 ) ) ;
#8042 = CARTESIAN_POINT ( 'NONE',  ( 2.500000000000000444, -1.035533905932737309, -1.049999997815050268 ) ) ;
#8043 = CARTESIAN_POINT ( 'NONE',  ( -5.558508435838188433, -2.857531096718932684, 5.000000000000004441 ) ) ;
#8044 = FACE_OUTER_BOUND ( 'NONE', #11642, .T. ) ;
#8045 = CARTESIAN_POINT ( 'NONE',  ( 1.767766952966368654, 1.767766952966369098, -0.8999999978150502455 ) ) ;
#8046 = CARTESIAN_POINT ( 'NONE',  ( -2.066987299999999639, 0.000000000000000000, -2.549999998907525711 ) ) ;
#8047 = DIRECTION ( 'NONE',  ( -0.000000000000000000, 1.000000000000000000, -0.000000000000000000 ) ) ;
#8048 = ADVANCED_FACE ( 'NONE', ( #15723 ), #13320, .F. ) ;
#8049 = EDGE_LOOP ( 'NONE', ( #9978, #7119, #6023, #5003 ) ) ;
#8050 = ORIENTED_EDGE ( 'NONE', *, *, #1073, .F. ) ;
#8051 = VERTEX_POINT ( 'NONE', #3615 ) ;
#8052 = CARTESIAN_POINT ( 'NONE',  ( 3.735808404764909163, -4.696639218303197083, 25.47398020122238904 ) ) ;
#8053 = CARTESIAN_POINT ( 'NONE',  ( 3.659182332138577465E-16, 214.7097693073062032, 7.296684523004520528 ) ) ;
#8054 = ORIENTED_EDGE ( 'NONE', *, *, #8359, .T. ) ;
#8055 = PRESENTATION_STYLE_ASSIGNMENT (( #5367 ) ) ;
#8056 = PRODUCT_DEFINITION_SHAPE ( 'NONE', 'NONE',  #15749 ) ;
#8057 = CARTESIAN_POINT ( 'NONE',  ( -1.035533905932737753, 2.500000000000000444, -0.7499999978150505564 ) ) ;
#8058 = CARTESIAN_POINT ( 'NONE',  ( -5.621278735166214346, -2.101423246382510879, 31.97408052783100985 ) ) ;
#8059 = CARTESIAN_POINT ( 'NONE',  ( 1.500000000000000000, 1.836970198721029934E-16, 2.500000000000000000 ) ) ;
#8060 = CARTESIAN_POINT ( 'NONE',  ( 1.461580736456473018, 184.5499999989075093, 5.538419263543527649 ) ) ;
#8061 = CARTESIAN_POINT ( 'NONE',  ( -2.500000000000000444, 1.035533905932737753, 2.456999999978150662 ) ) ;
#8062 = AXIS2_PLACEMENT_3D ( 'NONE', #2599, #218, #13496 ) ;
#8063 = CARTESIAN_POINT ( 'NONE',  ( -2.500000000000000444, 185.8999999978150584, 7.000000000000000000 ) ) ;
#8064 = CARTESIAN_POINT ( 'NONE',  ( 2.500000000000000444, 188.8499999999999659, 5.964466094067262247 ) ) ;
#8065 = CARTESIAN_POINT ( 'NONE',  ( 2.500000000000000000, 188.7199999975965738, 8.035533905932739529 ) ) ;
#8066 = CARTESIAN_POINT ( 'NONE',  ( 2.441738273555474681, 226.7282248110694809, 5.674544857840881029 ) ) ;
#8067 = DIRECTION ( 'NONE',  ( -0.5877852522924685852, -0.8090169943749508930, 0.000000000000000000 ) ) ;
#8068 = EDGE_LOOP ( 'NONE', ( #4235, #6767, #4811, #7637 ) ) ;
#8069 = CARTESIAN_POINT ( 'NONE',  ( 3.632753594129383146, -4.777047695050938181, 4.000049463537775907 ) ) ;
#8070 = EDGE_CURVE ( 'NONE', #5942, #567, #13748, .T. ) ;
#8071 = EDGE_CURVE ( 'NONE', #25, #15176, #11000, .T. ) ;
#8072 = VERTEX_POINT ( 'NONE', #2661 ) ;
#8073 = CARTESIAN_POINT ( 'NONE',  ( 2.996920846510591208, -5.485395142346733977, 5.614419472454843962 ) ) ;
#8074 = CIRCLE ( 'NONE', #1203, 12.49999999999999822 ) ;
#8075 = CARTESIAN_POINT ( 'NONE',  ( -3.000000000000000000, 1.732050807568877415, -5.500000000000000000 ) ) ;
#8076 = CARTESIAN_POINT ( 'NONE',  ( 6.176542424588109093, 0.9554180641286111886, 31.00000000000000000 ) ) ;
#8077 = EDGE_LOOP ( 'NONE', ( #10359, #5184 ) ) ;
#8078 = CARTESIAN_POINT ( 'NONE',  ( -5.935543223013842073, 0.8771126767608004027, 17.86760611998364823 ) ) ;
#8079 = EDGE_CURVE ( 'NONE', #5268, #13744, #1316, .T. ) ;
#8080 = CARTESIAN_POINT ( 'NONE',  ( 1.536366799937288086, 1.999167105995449445, -2.499999999999999556 ) ) ;
#8081 = CARTESIAN_POINT ( 'NONE',  ( -4.435347140101107755, -4.403429997944436458, 17.99999999999998934 ) ) ;
#8082 = CARTESIAN_POINT ( 'NONE',  ( 1.035533905932737531, 2.500000000000000444, -0.1499999999999999667 ) ) ;
#8083 = CARTESIAN_POINT ( 'NONE',  ( -2.668367453516648169, -5.373994336898122448, 31.13236078583911137 ) ) ;
#8084 = FILL_AREA_STYLE ('',( #757 ) ) ;
#8085 = CIRCLE ( 'NONE', #6573, 5.000000000000000000 ) ;
#8086 = CARTESIAN_POINT ( 'NONE',  ( 0.04609070931574436175, 0.4000000000000045186, -2.537007826417986944 ) ) ;
#8087 = CARTESIAN_POINT ( 'NONE',  ( 4.743384504624081899E-17, 185.6999999978150697, 4.500000000000000000 ) ) ;
#8088 = AXIS2_PLACEMENT_3D ( 'NONE', #4863, #3653, #7551 ) ;
#8089 = DIRECTION ( 'NONE',  ( 0.000000000000000000, 0.000000000000000000, 1.000000000000000000 ) ) ;
#8090 = CARTESIAN_POINT ( 'NONE',  ( -1.989902382949138460, 228.2815652486739282, 7.052567354366601649 ) ) ;
#8091 = DIRECTION ( 'NONE',  ( -1.000000000000000000, 0.000000000000000000, 0.000000000000000000 ) ) ;
#8092 = LINE ( 'NONE', #4270, #6462 ) ;
#8093 = CARTESIAN_POINT ( 'NONE',  ( -2.066987299999999639, 0.000000000000000000, -0.3499999989075254225 ) ) ;
#8094 = EDGE_CURVE ( 'NONE', #860, #13214, #11094, .T. ) ;
#8095 = CARTESIAN_POINT ( 'NONE',  ( 2.500000000000000000, 188.0000000000000000, 7.000000000000000000 ) ) ;
#8096 = DIRECTION ( 'NONE',  ( -6.123233995736766036E-17, 1.000000000000000000, 0.000000000000000000 ) ) ;
#8097 = EDGE_CURVE ( 'NONE', #6042, #7463, #2580, .T. ) ;
#8099 = VERTEX_POINT ( 'NONE', #9759 ) ;
#8098 = CARTESIAN_POINT ( 'NONE',  ( -2.500000000000000000, 0.000000000000000000, -1.399999997815050357 ) ) ;
#8100 = CARTESIAN_POINT ( 'NONE',  ( -5.615811513734980664, 2.743665920700508742, 18.50308643866043568 ) ) ;
#8101 = CARTESIAN_POINT ( 'NONE',  ( -1.084202172485504434E-16, 3.464101615137754830, -5.500000000000000000 ) ) ;
#8102 = CARTESIAN_POINT ( 'NONE',  ( -2.866366203691001147, 227.0037563968904237, 6.486100089110839129 ) ) ;
#8103 = SURFACE_STYLE_FILL_AREA ( #15656 ) ;
#8104 = CARTESIAN_POINT ( 'NONE',  ( 1.294034140306127068, 188.9999999982559586, 4.853059374542415760 ) ) ;
#8105 = DIRECTION ( 'NONE',  ( 0.9510565162951500895, 0.3090169943749582204, 0.000000000000000000 ) ) ;
#8106 = CARTESIAN_POINT ( 'NONE',  ( -1.990742470614812465, 228.3030780210874866, 7.114697468104904665 ) ) ;
#8107 = CARTESIAN_POINT ( 'NONE',  ( 1.924362066950147332, 228.0923243445923276, 6.506028829785237555 ) ) ;
#8109 = CARTESIAN_POINT ( 'NONE',  ( 6.155912734541126419, 1.081577393120926711, 10.99610786875027735 ) ) ;
#8108 = AXIS2_PLACEMENT_3D ( 'NONE', #12587, #8793, #342 ) ;
#8110 = CARTESIAN_POINT ( 'NONE',  ( 0.03853763818359707410, 0.4000000000000045186, 2.531640047765513213 ) ) ;
#8111 = B_SPLINE_CURVE_WITH_KNOTS ( 'NONE', 3,
 ( #10739, #10658, #15599, #7247, #13357, #2216, #10900, #11838, #4617, #7168, #4940, #7325, #6139, #12006, #15678, #5973, #1184, #10817 ),
 .UNSPECIFIED., .F., .F.,
 ( 4, 2, 2, 2, 2, 2, 2, 2, 4 ),
 ( 0.000000000000000000, 0.0003914898357794968989, 0.0007829796715589937978, 0.001174469507338490697, 0.001565959343117987596, 0.001957449178897484494, 0.002348939014676981393, 0.002740428850456478292, 0.003131918686235975191 ),
 .UNSPECIFIED. ) ;
#8112 = CARTESIAN_POINT ( 'NONE',  ( 0.6144377077730162062, 5.969178481556063787, 30.20033966857735663 ) ) ;
#8113 = ORIENTED_EDGE ( 'NONE', *, *, #4484, .T. ) ;
#8114 = CARTESIAN_POINT ( 'NONE',  ( -1.461580736456473684, 184.7499999989074979, 8.461580736456474128 ) ) ;
#8115 = CARTESIAN_POINT ( 'NONE',  ( 4.286401442266519091, 4.198423832313208592, 30.86763921416088863 ) ) ;
#8116 = ORIENTED_EDGE ( 'NONE', *, *, #12161, .T. ) ;
#8117 = FACE_OUTER_BOUND ( 'NONE', #10206, .T. ) ;
#8118 = CARTESIAN_POINT ( 'NONE',  ( 2.066987300000000083, 185.2499999989074979, 7.000000000000000000 ) ) ;
#8119 = CARTESIAN_POINT ( 'NONE',  ( 3.882809187878849322, 4.899079348630116293, 17.02599901976669017 ) ) ;
#8120 = CARTESIAN_POINT ( 'NONE',  ( -4.811147140404425926E-16, 185.6499999989075320, 9.066987300000000971 ) ) ;
#8121 = CARTESIAN_POINT ( 'NONE',  ( -0.8738043859789326184, 6.188821459035897199, 25.00341560223737503 ) ) ;
#8122 = CARTESIAN_POINT ( 'NONE',  ( -1.035533905932738197, -2.500000000000000000, 0.3500000021849497545 ) ) ;
#8123 = CARTESIAN_POINT ( 'NONE',  ( 4.195842658231499378, -4.289229542213141677, 10.99560239355786173 ) ) ;
#8124 = CARTESIAN_POINT ( 'NONE',  ( 0.000000000000000000, 215.7452399395091049, 13.29567785264566027 ) ) ;
#8125 = CARTESIAN_POINT ( 'NONE',  ( -1.035533905932737975, 188.9499999978150129, 4.500000000000001776 ) ) ;
#8126 = CARTESIAN_POINT ( 'NONE',  ( -5.903057025253884760, -1.078199533779625963, 17.38438267301393481 ) ) ;
#8127 = CARTESIAN_POINT ( 'NONE',  ( -0.07717340183324797320, 189.6978550888158281, 10.38866401756451552 ) ) ;
#8128 =( REPRESENTATION_RELATIONSHIP ('NONE','NONE', #11191, #9569 ) REPRESENTATION_RELATIONSHIP_WITH_TRANSFORMATION ( #1754 )SHAPE_REPRESENTATION_RELATIONSHIP( ) );
#8129 = EDGE_LOOP ( 'NONE', ( #14333, #7162, #243, #6480 ) ) ;
#8130 = VERTEX_POINT ( 'NONE', #3692 ) ;
#8131 = EDGE_LOOP ( 'NONE', ( #411, #8315, #7275, #11981 ) ) ;
#8132 = CARTESIAN_POINT ( 'NONE',  ( 4.344265632482128048, -4.493596842504916644, 12.00425949503009093 ) ) ;
#8133 = FACE_OUTER_BOUND ( 'NONE', #13580, .T. ) ;
#8134 = EDGE_LOOP ( 'NONE', ( #698, #6463, #2210, #12366 ) ) ;
#8135 = CARTESIAN_POINT ( 'NONE',  ( 1.767766952966369320, -1.767766952966368654, -1.099999997815050534 ) ) ;
#8136 = ADVANCED_FACE ( 'NONE', ( #12205 ), #11015, .T. ) ;
#8137 = EDGE_CURVE ( 'NONE', #13466, #4492, #7438, .T. ) ;
#8138 = CARTESIAN_POINT ( 'NONE',  ( -5.317509234263920526, -2.779225709351067053, 31.00000000000000000 ) ) ;
#8139 = AXIS2_PLACEMENT_3D ( 'NONE', #4982, #3771, #12128 ) ;
#8140 = CARTESIAN_POINT ( 'NONE',  ( 4.435347140100866170, 4.403429997944679819, 24.49999999999999289 ) ) ;
#8141 = CARTESIAN_POINT ( 'NONE',  ( 1.767766952966369098, 189.5999999978150470, 5.232233047033630235 ) ) ;
#8142 = CARTESIAN_POINT ( 'NONE',  ( 1.035533905932739085, -2.500000000000000000, 1.156999999978150395 ) ) ;
#8143 = EDGE_CURVE ( 'NONE', #3740, #13757, #1808, .T. ) ;
#8144 = DIRECTION ( 'NONE',  ( 0.8660254037844503650, -0.4999999999999796829, -0.000000000000000000 ) ) ;
#8145 = APPLICATION_PROTOCOL_DEFINITION ( 'draft international standard', 'automotive_design', 1998, #4761 ) ;
#8146 = CARTESIAN_POINT ( 'NONE',  ( -2.066987299999999639, 0.8561741729129452860, 2.000000001092474555 ) ) ;
#8147 = LINE ( 'NONE', #5683, #7833 ) ;
#8148 = CARTESIAN_POINT ( 'NONE',  ( 0.9678947859540896204, 226.3761757439112898, 4.637006245081842337 ) ) ;
#8149 = CARTESIAN_POINT ( 'NONE',  ( 2.817313151350985034, 5.579000502529535943, 18.13063932754211649 ) ) ;
#8150 = B_SPLINE_CURVE_WITH_KNOTS ( 'NONE', 3,
 ( #1287, #99, #13304, #8226, #7271, #4884, #13227, #6161, #5917, #15701, #973, #4723, #7032, #4966, #10764, #2241, #7112, #11948 ),
 .UNSPECIFIED., .F., .F.,
 ( 4, 2, 2, 2, 2, 2, 2, 2, 4 ),
 ( 0.000000000000000000, 0.0003914357524127478108, 0.0007828715048254956217, 0.001174307257238243378, 0.001565743009650992328, 0.001957178762063741060, 0.002348614514476489792, 0.002740050266889238959, 0.003131486019301987257 ),
 .UNSPECIFIED. ) ;
#8151 = ORIENTED_EDGE ( 'NONE', *, *, #5529, .F. ) ;
#8152 = CARTESIAN_POINT ( 'NONE',  ( -5.317509234263873452, 2.779225709351156315, 24.63061695532138629 ) ) ;
#8153 = ORIENTED_EDGE ( 'NONE', *, *, #364, .F. ) ;
#8154 = CARTESIAN_POINT ( 'NONE',  ( 0.000000000000000000, 6.250000000000000888, 12.49999999999998401 ) ) ;
#8155 = CARTESIAN_POINT ( 'NONE',  ( 4.142173849413723907, -4.341773579105426606, 17.38480617551147844 ) ) ;
#8156 = CARTESIAN_POINT ( 'NONE',  ( 5.570760634536855882, 2.834026536768143423, 24.23774718278285789 ) ) ;
#8157 = EDGE_LOOP ( 'NONE', ( #10056, #2772, #8212, #9421 ) ) ;
#8158 = CARTESIAN_POINT ( 'NONE',  ( 3.253823204785082357, 5.337590213880527124, 10.62694108445697339 ) ) ;
#8159 = CARTESIAN_POINT ( 'NONE',  ( 0.000000000000000000, 19.99999999999999645, -7.000000000000000000 ) ) ;
#8160 = CARTESIAN_POINT ( 'NONE',  ( -3.159082487394832217, -5.393634094348301211, 18.79954462468841569 ) ) ;
#8161 = CARTESIAN_POINT ( 'NONE',  ( 1.767766952966368654, 1.767766952966369098, -1.000000000000000000 ) ) ;
#8162 = CARTESIAN_POINT ( 'NONE',  ( 0.000000000000000000, -0.3999999999999941380, 2.450963827680237017 ) ) ;
#8163 = SURFACE_STYLE_USAGE ( .BOTH. , #2261 ) ;
#8164 = CARTESIAN_POINT ( 'NONE',  ( -0.001074311305641557088, 226.3251817249170017, 4.486671161788877704 ) ) ;
#8165 = CARTESIAN_POINT ( 'NONE',  ( 1.035533905932738419, 186.1499999978150584, 9.500000000000003553 ) ) ;
#8166 = B_SPLINE_CURVE_WITH_KNOTS ( 'NONE', 3,
 ( #60, #4926, #13427, #9781, #14627, #3716, #3946, #2922, #10245, #11274, #8820, #12383, #13650, #12698, #9061, #5241, #12543, #7619 ),
 .UNSPECIFIED., .F., .F.,
 ( 4, 2, 2, 2, 2, 2, 2, 2, 4 ),
 ( 0.000000000000000000, 0.0003914357524127498708, 0.0007828715048254997417, 0.001174307257238249667, 0.001565743009650999483, 0.001957178762063747999, 0.002348614514476496298, 0.002740050266889245030, 0.003131486019301993329 ),
 .UNSPECIFIED. ) ;
#8167 = CARTESIAN_POINT ( 'NONE',  ( -0.3256308520141213414, 228.9034500205340237, 8.848606045481535176 ) ) ;
#8168 = CARTESIAN_POINT ( 'NONE',  ( 5.486982057989171047, 2.429327048029922942, 10.70068193741825802 ) ) ;
#8169 = CARTESIAN_POINT ( 'NONE',  ( -5.409007216690653763, 2.598315788643790203, 18.61442521571937192 ) ) ;
#8170 = CARTESIAN_POINT ( 'NONE',  ( -0.8561741729129458411, -2.066987299999999195, -0.9999999989075253337 ) ) ;
#8171 = CARTESIAN_POINT ( 'NONE',  ( 2.500000000000000444, 186.4000000000000057, 7.000000000000000000 ) ) ;
#8172 = CARTESIAN_POINT ( 'NONE',  ( -4.291255145204205590, 4.544933371694557245, 25.11396179408071205 ) ) ;
#8173 = B_SPLINE_CURVE_WITH_KNOTS ( 'NONE', 3,
 ( #15597, #4698, #3105, #11836, #6288, #13202, #3572, #7396, #14475, #8362, #8443, #10973, #2378, #1413, #13279, #13509, #9867, #6054 ),
 .UNSPECIFIED., .F., .F.,
 ( 4, 2, 2, 2, 2, 2, 2, 2, 4 ),
 ( 0.003131490185286017660, 0.003522829482338626830, 0.003914168779391236433, 0.004305508076443845603, 0.004696847373496454772, 0.005088186670549063942, 0.005479525967601673112, 0.005870865264654282281, 0.006262204561706891451 ),
 .UNSPECIFIED. ) ;
#8175 = EDGE_LOOP ( 'NONE', ( #5901, #13759 ) ) ;
#8174 = CARTESIAN_POINT ( 'NONE',  ( 0.000000000000000000, 0.000000000000000000, 2.500000000000000000 ) ) ;
#8176 = EDGE_CURVE ( 'NONE', #12135, #10533, #12516, .T. ) ;
#8177 = CARTESIAN_POINT ( 'NONE',  ( -6.081509788407727157, 1.446521464462764417, 18.87381964045070859 ) ) ;
#8178 = ORIENTED_EDGE ( 'NONE', *, *, #4656, .F. ) ;
#8179 = B_SPLINE_CURVE_WITH_KNOTS ( 'NONE', 3,
 ( #13974, #11584, #6751, #6673, #682, #3230, #3312, #7929, #11743, #15496, #7861, #1876, #5633, #8172, #13012, #5555, #14048, #2112 ),
 .UNSPECIFIED., .F., .F.,
 ( 4, 2, 2, 2, 2, 2, 2, 2, 4 ),
 ( 0.000000000000000000, 0.0003914357524127493287, 0.0007828715048254986575, 0.001174307257238248149, 0.001565743009650997315, 0.001957178762063746698, 0.002348614514476494563, 0.002740050266889243295, 0.003131486019301991160 ),
 .UNSPECIFIED. ) ;
#8180 = CARTESIAN_POINT ( 'NONE',  ( -5.935543223013831415, 0.8771126767608680153, 24.49999999999999289 ) ) ;
#8181 = CARTESIAN_POINT ( 'NONE',  ( -2.770343633091874036, 227.6599362732561644, 8.417748511065344275 ) ) ;
#8182 = ADVANCED_FACE ( 'NONE', ( #8958 ), #10065, .F. ) ;
#8183 = CARTESIAN_POINT ( 'NONE',  ( 2.500000000000000444, 186.4000000000000057, 7.000000000000000000 ) ) ;
#8184 = CARTESIAN_POINT ( 'NONE',  ( 1.035533905932738419, 185.3800000002184731, 9.500000000000003553 ) ) ;
#8185 = DIRECTION ( 'NONE',  ( 0.000000000000000000, 0.000000000000000000, -1.000000000000000000 ) ) ;
#8186 = CARTESIAN_POINT ( 'NONE',  ( 1.886647494277889692, 228.0514830721454871, 6.388076905524764371 ) ) ;
#8187 = CARTESIAN_POINT ( 'NONE',  ( 6.081590040723071411, 1.446205118473034013, 10.62632671364004722 ) ) ;
#8188 = CARTESIAN_POINT ( 'NONE',  ( 5.131373506000491247, 7.062729720844170167, 17.99999999999998934 ) ) ;
#8189 = AXIS2_PLACEMENT_3D ( 'NONE', #9692, #9611, #14531 ) ;
#8190 = CARTESIAN_POINT ( 'NONE',  ( 2.094888807778566729E-14, 6.000000000000000888, 30.00000000000000000 ) ) ;
#8191 = ADVANCED_FACE ( 'NONE', ( #2898 ), #14821, .T. ) ;
#8192 = ORIENTED_EDGE ( 'NONE', *, *, #5424, .T. ) ;
#8193 = CARTESIAN_POINT ( 'NONE',  ( 1.461580736456472351, 189.1499999989075320, 8.461580736456474128 ) ) ;
#8194 = PRODUCT_DEFINITION_SHAPE ( 'NONE', 'NONE',  #15740 ) ;
#8195 = CARTESIAN_POINT ( 'NONE',  ( -0.7993282387950335632, 5.947240459526521583, 12.11484358216956991 ) ) ;
#8196 = ORIENTED_EDGE ( 'NONE', *, *, #10028, .F. ) ;
#8197 = DIRECTION ( 'NONE',  ( -0.3090169943749446202, -0.9510565162951544194, 0.000000000000000000 ) ) ;
#8198 = CIRCLE ( 'NONE', #3103, 1.500000000000001776 ) ;
#8199 = CARTESIAN_POINT ( 'NONE',  ( 0.8561741729129455081, 185.3999999989075604, 4.933012699999999029 ) ) ;
#8200 = DIRECTION ( 'NONE',  ( 1.062480551894329776E-17, 2.775557561562888393E-16, -1.000000000000000000 ) ) ;
#8201 = CARTESIAN_POINT ( 'NONE',  ( 2.066987300000000083, 187.3999999989075320, 7.856174172912946396 ) ) ;
#8202 = FACE_BOUND ( 'NONE', #14381, .T. ) ;
#8203 = CARTESIAN_POINT ( 'NONE',  ( -2.500000000000000444, 1.035533905932737753, 0.1500000021849498544 ) ) ;
#8204 = CARTESIAN_POINT ( 'NONE',  ( -5.648794263291753381, -2.676232015153594102, 4.385580527545152485 ) ) ;
#8205 = CARTESIAN_POINT ( 'NONE',  ( -5.999999999999999112, 201.6409668649147022, 13.30942870683726120 ) ) ;
#8206 = CARTESIAN_POINT ( 'NONE',  ( 0.5043776560897653694, -6.230795654995838539, 31.87337476296011474 ) ) ;
#8207 = CARTESIAN_POINT ( 'NONE',  ( 2.066987299999999639, 0.8561741729129456191, -2.099999998907525534 ) ) ;
#8208 = CARTESIAN_POINT ( 'NONE',  ( 5.843318061569051203, 1.367618216965616362, 12.37303779027049089 ) ) ;
#8209 = ORIENTED_EDGE ( 'NONE', *, *, #5529, .T. ) ;
#8210 = VECTOR ( 'NONE', #12978, 1000.000000000000000 ) ;
#8211 = ORIENTED_EDGE ( 'NONE', *, *, #10754, .T. ) ;
#8212 = ORIENTED_EDGE ( 'NONE', *, *, #4484, .F. ) ;
#8213 = CARTESIAN_POINT ( 'NONE',  ( 2.066987300000000083, 184.4999999989074979, 6.143825827087054492 ) ) ;
#8214 = FACE_OUTER_BOUND ( 'NONE', #1664, .T. ) ;
#8215 = ORIENTED_EDGE ( 'NONE', *, *, #14278, .T. ) ;
#8216 = CARTESIAN_POINT ( 'NONE',  ( 1.767766952966368654, 1.767766952966369098, -2.499999997815050445 ) ) ;
#8217 = CARTESIAN_POINT ( 'NONE',  ( -0.5044069930201257046, 5.979990686695010105, 25.37335743227903606 ) ) ;
#8218 = CARTESIAN_POINT ( 'NONE',  ( -4.435347140101012720, -4.403429997944533270, 4.869360672457872852 ) ) ;
#8219 = CARTESIAN_POINT ( 'NONE',  ( -1.035533905932737975, 188.1499999978150868, 4.500000000000000888 ) ) ;
#8220 = VECTOR ( 'NONE', #13903, 1000.000000000000114 ) ;
#8221 = CARTESIAN_POINT ( 'NONE',  ( -2.500000000000000000, -1.035533905932739307, 0.9569999999781505506 ) ) ;
#8222 = ADVANCED_BREP_SHAPE_REPRESENTATION ( '', ( #10455, #14201 ), #4310 ) ;
#8223 = CARTESIAN_POINT ( 'NONE',  ( 6.143020266950980357, -1.155160780047701508, 4.385580527545153373 ) ) ;
#8224 = CONTEXT_DEPENDENT_SHAPE_REPRESENTATION ( #4550, #9462 ) ;
#8225 = CARTESIAN_POINT ( 'NONE',  ( -2.066987299999999195, -0.8561741729129466183, -0.2999999989075253226 ) ) ;
#8226 = CARTESIAN_POINT ( 'NONE',  ( 4.344313232727158969, -4.493553492990063347, 30.49563030319846391 ) ) ;
#8227 = CARTESIAN_POINT ( 'NONE',  ( 1.829800800964088481, 226.5245823332902546, 5.074452397578279594 ) ) ;
#8228 = CARTESIAN_POINT ( 'NONE',  ( -9.750000000000003553, 184.0000000000000000, -3.401296724241641415E-14 ) ) ;
#8229 = ORIENTED_EDGE ( 'NONE', *, *, #8923, .T. ) ;
#8230 = CARTESIAN_POINT ( 'NONE',  ( -5.531209434046284734, 2.328189801702745587, 25.37303779027051220 ) ) ;
#8231 = VERTEX_POINT ( 'NONE', #5296 ) ;
#8232 = CIRCLE ( 'NONE', #849, 1.999999999999999556 ) ;
#8233 = VERTEX_POINT ( 'NONE', #14914 ) ;
#8234 = EDGE_CURVE ( 'NONE', #5635, #1447, #15069, .T. ) ;
#8235 = CARTESIAN_POINT ( 'NONE',  ( -6.105861027178947076, -1.337741388556997313, 30.20045537531156654 ) ) ;
#8236 = CARTESIAN_POINT ( 'NONE',  ( 0.5039005892421229982, -6.230833003620540822, 4.126363889112978356 ) ) ;
#8237 = VERTEX_POINT ( 'NONE', #13862 ) ;
#8238 = CARTESIAN_POINT ( 'NONE',  ( -5.375763363753407909, 2.665284979407616550, 17.49610204984017159 ) ) ;
#8239 = DIRECTION ( 'NONE',  ( 0.000000000000000000, 0.000000000000000000, -1.000000000000000000 ) ) ;
#8240 = CARTESIAN_POINT ( 'NONE',  ( -0.1306070469491344976, -6.250000000000003553, 23.49999999999998934 ) ) ;
#8241 = DIRECTION ( 'NONE',  ( 0.000000000000000000, 0.000000000000000000, 1.000000000000000000 ) ) ;
#8242 = CARTESIAN_POINT ( 'NONE',  ( -5.558508435838095174, -2.857531096719115649, 24.49999999999999289 ) ) ;
#8243 = CARTESIAN_POINT ( 'NONE',  ( 2.030576276931546336E-13, -6.000000000000000888, 25.49999999999999645 ) ) ;
#8244 =( LENGTH_UNIT ( ) NAMED_UNIT ( * ) SI_UNIT ( .MILLI., .METRE. ) );
#8245 = DIRECTION ( 'NONE',  ( 0.000000000000000000, 0.000000000000000000, -1.000000000000000000 ) ) ;
#8246 = CARTESIAN_POINT ( 'NONE',  ( -1.035533905932739751, 187.7500000000000284, 9.500000000000003553 ) ) ;
#8247 = CARTESIAN_POINT ( 'NONE',  ( -1.160340649284625325, 228.7901875120212196, 8.521497460825987247 ) ) ;
#8248 = CARTESIAN_POINT ( 'NONE',  ( -6.155867707731084160, -1.081837891426048248, 18.50436969680152899 ) ) ;
#8249 = EDGE_CURVE ( 'NONE', #15136, #1178, #3878, .T. ) ;
#8250 = CARTESIAN_POINT ( 'NONE',  ( 5.915755444410793373, 1.003187219519900752, 31.50312048902375395 ) ) ;
#8251 = ORIENTED_EDGE ( 'NONE', *, *, #11861, .T. ) ;
#8252 = CARTESIAN_POINT ( 'NONE',  ( -1.084202172485504434E-15, -3.464101615137755275, -2.500000000000000000 ) ) ;
#8254 = ORIENTED_EDGE ( 'NONE', *, *, #160, .T. ) ;
#8253 = DIRECTION ( 'NONE',  ( 0.000000000000000000, 1.000000000000000000, 0.000000000000000000 ) ) ;
#8255 = DIRECTION ( 'NONE',  ( 0.000000000000000000, 1.000000000000000000, 0.000000000000000000 ) ) ;
#8256 = DIRECTION ( 'NONE',  ( 0.8090169943749421222, 0.5877852522924802425, 0.000000000000000000 ) ) ;
#8257 = VECTOR ( 'NONE', #8304, 1000.000000000000000 ) ;
#8258 = CARTESIAN_POINT ( 'NONE',  ( 1.767766952966369098, 186.5000000000000000, 5.232233047033630235 ) ) ;
#8259 = CARTESIAN_POINT ( 'NONE',  ( -2.687528980000447820, 226.8550369918930869, 6.048145777815692625 ) ) ;
#8260 = CARTESIAN_POINT ( 'NONE',  ( 5.571002711501470195, 2.833546409886167350, 24.76379616840807074 ) ) ;
#8261 = EDGE_CURVE ( 'NONE', #8538, #4157, #9601, .T. ) ;
#8262 = CARTESIAN_POINT ( 'NONE',  ( 2.500000000000000444, 184.7800000002184788, 5.964466094067262247 ) ) ;
#8263 = DIRECTION ( 'NONE',  ( -1.000000000000000000, 0.000000000000000000, 0.000000000000000000 ) ) ;
#8264 = CARTESIAN_POINT ( 'NONE',  ( -1.212146835196386663, 227.7435586823976337, 5.498773705076675178 ) ) ;
#8265 = FACE_BOUND ( 'NONE', #13703, .T. ) ;
#8266 = B_SPLINE_CURVE_WITH_KNOTS ( 'NONE', 3,
 ( #5640, #11593, #6607, #855, #5721, #15420, #2938, #10491, #12632, #1731, #12711, #11679, #1810, #541, #617, #15262, #5489, #5410 ),
 .UNSPECIFIED., .F., .F.,
 ( 4, 2, 2, 2, 2, 2, 2, 2, 4 ),
 ( 0.000000000000000000, 0.0003914904498596298880, 0.0007829808997192597760, 0.001174471349578889772, 0.001565961799438519552, 0.001957452249298139140, 0.002348942699157758728, 0.002740433149017377883, 0.003131923598876997471 ),
 .UNSPECIFIED. ) ;
#8267 = CARTESIAN_POINT ( 'NONE',  ( -1.461580736456472351, -1.461580736456473018, -0.8499999989075254225 ) ) ;
#8268 = CARTESIAN_POINT ( 'NONE',  ( -3.061616997868391523E-16, 189.0000000000000000, 9.500000000000000000 ) ) ;
#8269 = ORIENTED_EDGE ( 'NONE', *, *, #10673, .T. ) ;
#8270 = CARTESIAN_POINT ( 'NONE',  ( 2.066987300000000083, 188.2999999989075093, 6.143825827087054492 ) ) ;
#8271 = CARTESIAN_POINT ( 'NONE',  ( -0.1306497350716639139, 6.000000000000002665, 10.49999999999998224 ) ) ;
#8272 = STYLED_ITEM ( 'NONE', ( #3806 ), #10345 ) ;
#8273 = VERTEX_POINT ( 'NONE', #651 ) ;
#8274 = EDGE_CURVE ( 'NONE', #15705, #860, #11862, .T. ) ;
#8275 = EDGE_CURVE ( 'NONE', #5575, #8394, #736, .T. ) ;
#8276 = PLANE ( 'NONE',  #1498 ) ;
#8277 = CARTESIAN_POINT ( 'NONE',  ( -4.005361199355036206, 4.468319061418737803, 31.80022217383877248 ) ) ;
#8278 = CARTESIAN_POINT ( 'NONE',  ( -2.668367453516768517, 5.373994336898062052, 11.49999999999998224 ) ) ;
#8279 = EDGE_CURVE ( 'NONE', #6298, #13830, #15540, .T. ) ;
#8280 = CARTESIAN_POINT ( 'NONE',  ( 2.066987300000000083, 185.7999999989075093, 7.856174172912946396 ) ) ;
#8281 = CARTESIAN_POINT ( 'NONE',  ( 3.312524433819702185, 5.004191858254053216, 18.97408052783099563 ) ) ;
#8282 = CARTESIAN_POINT ( 'NONE',  ( 2.500000000000000000, 3.061616997868383141E-16, -0.9999999978150501123 ) ) ;
#8283 = CARTESIAN_POINT ( 'NONE',  ( 2.848235266351003325, -5.281699484015657475, 10.88602261056917442 ) ) ;
#8284 = CARTESIAN_POINT ( 'NONE',  ( 0.000000000000000000, 185.8606548077538321, 9.048340948986950849 ) ) ;
#8285 = CARTESIAN_POINT ( 'NONE',  ( 0.8736772044960189332, -6.188841968496057611, 30.49611573292811428 ) ) ;
#8286 = CARTESIAN_POINT ( 'NONE',  ( -1.035533905932739529, 185.2499999978150811, 9.500000000000000000 ) ) ;
#8287 = CARTESIAN_POINT ( 'NONE',  ( -0.5031281619706412522, -5.980084330432680950, 17.12602272744524257 ) ) ;
#8288 = ORIENTED_EDGE ( 'NONE', *, *, #4957, .T. ) ;
#8289 = VERTEX_POINT ( 'NONE', #9570 ) ;
#8290 = EDGE_LOOP ( 'NONE', ( #1038, #1350, #11139, #14035 ) ) ;
#8291 = CARTESIAN_POINT ( 'NONE',  ( 2.930600586412946740, 5.520563544161762870, 30.49691356133955011 ) ) ;
#8292 = DIRECTION ( 'NONE',  ( -6.123233995736766036E-17, 1.000000000000000000, 0.000000000000000000 ) ) ;
#8293 = ORIENTED_EDGE ( 'NONE', *, *, #8473, .F. ) ;
#8294 = EDGE_CURVE ( 'NONE', #7182, #14655, #1338, .T. ) ;
#8295 = CARTESIAN_POINT ( 'NONE',  ( -1.035533905932737753, 2.500000000000000444, -2.349999997815050090 ) ) ;
#8296 = CARTESIAN_POINT ( 'NONE',  ( 0.8737888311110059147, -5.936248257219507884, 5.503441851412170571 ) ) ;
#8297 = CARTESIAN_POINT ( 'NONE',  ( 4.153663429050612699, 4.670992970568521585, 25.29933148907577944 ) ) ;
#8298 = CARTESIAN_POINT ( 'NONE',  ( -2.066987300000001415, 188.0999999989074922, 7.856174172912944620 ) ) ;
#8299 = CARTESIAN_POINT ( 'NONE',  ( 4.592425496802573972E-16, -2.500000000000000000, 1.106999999978150573 ) ) ;
#8300 = LINE ( 'NONE', #6799, #9985 ) ;
#8301 = CARTESIAN_POINT ( 'NONE',  ( 0.8561741729129451750, 2.066987299999999639, 1.800000001092475266 ) ) ;
#8302 = CARTESIAN_POINT ( 'NONE',  ( 3.459597053047918980, -5.206576120509697425, 4.025914576658297328 ) ) ;
#8303 = CARTESIAN_POINT ( 'NONE',  ( 2.383228694455616914, 226.7027912316577556, 5.599607710487992662 ) ) ;
#8304 = DIRECTION ( 'NONE',  ( 0.000000000000000000, 1.000000000000000000, 0.000000000000000000 ) ) ;
#8305 = ORIENTED_EDGE ( 'NONE', *, *, #15480, .F. ) ;
#8306 = B_SPLINE_CURVE_WITH_KNOTS ( 'NONE', 3,
 ( #4861, #13115, #2380, #4779, #1263, #3334, #6056, #1028, #14390, #11923, #8281, #4700, #2462, #1109, #9470, #12085, #9552, #7087 ),
 .UNSPECIFIED., .F., .F.,
 ( 4, 2, 2, 2, 2, 2, 2, 2, 4 ),
 ( 0.000000000000000000, 0.0003914898357794968447, 0.0007829796715589936893, 0.001174469507338490480, 0.001565959343117987379, 0.001957449178897484061, 0.002348939014676980960, 0.002740428850456477858, 0.003131918686235974757 ),
 .UNSPECIFIED. ) ;
#8307 = ORIENTED_EDGE ( 'NONE', *, *, #9282, .F. ) ;
#8308 = DIRECTION ( 'NONE',  ( 0.000000000000000000, 0.000000000000000000, -1.000000000000000000 ) ) ;
#8309 = ORIENTED_EDGE ( 'NONE', *, *, #12525, .F. ) ;
#8310 = ORIENTED_EDGE ( 'NONE', *, *, #12029, .T. ) ;
#8311 = CARTESIAN_POINT ( 'NONE',  ( 0.1306070469493592900, 6.250000000000000000, 29.99999999999999289 ) ) ;
#8312 = EDGE_CURVE ( 'NONE', #7910, #2947, #8300, .T. ) ;
#8313 = CARTESIAN_POINT ( 'NONE',  ( -2.997451966578516203, -5.485105005465951145, 23.88482219624157210 ) ) ;
#8314 = CARTESIAN_POINT ( 'NONE',  ( -4.267838854167235851, -4.217593933790273475, 24.76239891805597182 ) ) ;
#8315 = ORIENTED_EDGE ( 'NONE', *, *, #6913, .T. ) ;
#8316 = CARTESIAN_POINT ( 'NONE',  ( -6.172552660730993068, 0.9821660343537826909, 31.26379616840805653 ) ) ;
#8317 = CARTESIAN_POINT ( 'NONE',  ( -0.5042675786779248215, -6.230788509548839116, 5.873310683104476126 ) ) ;
#8318 = FACE_BOUND ( 'NONE', #11684, .T. ) ;
#8319 = CARTESIAN_POINT ( 'NONE',  ( 1.035533905932739085, -2.500000000000000000, -1.149999997815050135 ) ) ;
#8320 = CARTESIAN_POINT ( 'NONE',  ( 5.317509234263941842, 2.779225709351030638, 31.00000000000000000 ) ) ;
#8321 = DIRECTION ( 'NONE',  ( -0.3090169943749584425, 0.9510565162951498674, 0.000000000000000000 ) ) ;
#8322 =( NAMED_UNIT ( * ) SI_UNIT ( $, .STERADIAN. ) SOLID_ANGLE_UNIT ( ) );
#8323 = PRODUCT_DEFINITION_SHAPE ( 'NONE', 'NONE',  #15755 ) ;
#8324 = CARTESIAN_POINT ( 'NONE',  ( 1.035533905932737753, 189.6499999978150868, 4.500000000000000888 ) ) ;
#8325 = CARTESIAN_POINT ( 'NONE',  ( -0.1300625424525254092, 228.9108363453237303, 8.869938172763147222 ) ) ;
#8326 = CARTESIAN_POINT ( 'NONE',  ( 3.632753594129297880, 4.777047695051003018, 31.99995053646222942 ) ) ;
#8327 = CIRCLE ( 'NONE', #688, 1.499999999999999556 ) ;
#8328 = CARTESIAN_POINT ( 'NONE',  ( 5.783198643800752770, 1.602922020054757590, 31.97377823943293151 ) ) ;
#8329 = EDGE_LOOP ( 'NONE', ( #9321, #6867 ) ) ;
#8330 = CARTESIAN_POINT ( 'NONE',  ( -5.782947755040664717, 1.603807858343995640, 12.47398020122238194 ) ) ;
#8331 = CARTESIAN_POINT ( 'NONE',  ( -0.6156307853268694341, -5.969051238897262301, 12.29870573410680201 ) ) ;
#8333 = EDGE_LOOP ( 'NONE', ( #15336, #4334, #239, #15665 ) ) ;
#8332 = CARTESIAN_POINT ( 'NONE',  ( 5.621197618055745693, 2.101623592078328162, 25.47398020122238194 ) ) ;
#8334 = DIRECTION ( 'NONE',  ( 0.000000000000000000, 0.000000000000000000, -1.000000000000000000 ) ) ;
#8335 = FACE_OUTER_BOUND ( 'NONE', #1351, .T. ) ;
#8336 = ORIENTED_EDGE ( 'NONE', *, *, #14100, .F. ) ;
#8337 = AXIS2_PLACEMENT_3D ( 'NONE', #7878, #12719, #5343 ) ;
#8338 = CARTESIAN_POINT ( 'NONE',  ( -4.142620314836288564, -4.341347824677590950, 5.614425215719389683 ) ) ;
#8339 =( REPRESENTATION_RELATIONSHIP ('NONE','NONE', #11191, #4596 ) REPRESENTATION_RELATIONSHIP_WITH_TRANSFORMATION ( #4145 )SHAPE_REPRESENTATION_RELATIONSHIP( ) );
#8340 = CARTESIAN_POINT ( 'NONE',  ( -2.066987299999999195, -0.8561741729129466183, 0.7000000010924749549 ) ) ;
#8341 = CARTESIAN_POINT ( 'NONE',  ( -2.126963226675738117, 226.6093206107916274, 5.324180815053653149 ) ) ;
#8342 = EDGE_CURVE ( 'NONE', #278, #5925, #9491, .T. ) ;
#8343 = CARTESIAN_POINT ( 'NONE',  ( 1.074754184052031381, 190.0681451684283729, 4.397840615916859264 ) ) ;
#8344 = CARTESIAN_POINT ( 'NONE',  ( -1.767766952966369765, 187.6300000002185016, 8.767766952966368876 ) ) ;
#8345 = CARTESIAN_POINT ( 'NONE',  ( -2.897581130414634077E-17, 22.00000000000000000, -8.250000000000003553 ) ) ;
#8346 = ADVANCED_FACE ( 'NONE', ( #7982 ), #15461, .F. ) ;
#8347 = CARTESIAN_POINT ( 'NONE',  ( 1.161994134746590523, 227.7310455073454136, 5.462634941821782775 ) ) ;
#8348 = CARTESIAN_POINT ( 'NONE',  ( -5.558508435838126260, -2.857531096719055252, 17.99999999999998934 ) ) ;
#8349 = CARTESIAN_POINT ( 'NONE',  ( -2.066987299999999639, 0.8561741729129455081, 1.400000001092474911 ) ) ;
#8350 = CARTESIAN_POINT ( 'NONE',  ( 1.767766952966368654, 1.767766952966369098, 1.399999999999999911 ) ) ;
#8351 = EDGE_CURVE ( 'NONE', #14543, #14401, #14034, .T. ) ;
#8352 = VERTEX_POINT ( 'NONE', #9259 ) ;
#8353 = CARTESIAN_POINT ( 'NONE',  ( -0.8561741729129458411, 187.6999999989075150, 4.933012699999999029 ) ) ;
#8354 = AXIS2_PLACEMENT_3D ( 'NONE', #9997, #7445, #12289 ) ;
#8355 = CARTESIAN_POINT ( 'NONE',  ( -2.066987300000001415, 186.2999999989075093, 7.856174172912944620 ) ) ;
#8356 = CARTESIAN_POINT ( 'NONE',  ( 5.903347812666377870, 1.076697810262441823, 23.88602261056918152 ) ) ;
#8357 = ORIENTED_EDGE ( 'NONE', *, *, #3306, .F. ) ;
#8358 = CARTESIAN_POINT ( 'NONE',  ( -2.500000000000000444, 186.0000000000000000, 7.000000000000000000 ) ) ;
#8359 = EDGE_CURVE ( 'NONE', #5418, #2406, #2951, .T. ) ;
#8360 = CARTESIAN_POINT ( 'NONE',  ( 5.782895619916165408, -1.604017620858050330, 5.974080527831013399 ) ) ;
#8361 = CARTESIAN_POINT ( 'NONE',  ( 0.000000000000000000, 0.000000000000000000, 52.97056274847714263 ) ) ;
#8362 = CARTESIAN_POINT ( 'NONE',  ( 1.000082492230778053, 6.169467968613697728, 11.63152538105394740 ) ) ;
#8363 = CARTESIAN_POINT ( 'NONE',  ( 0.8561741729129460632, 187.2999999989075661, 9.066987300000000971 ) ) ;
#8364 = VECTOR ( 'NONE', #3443, 1000.000000000000000 ) ;
#8365 = CARTESIAN_POINT ( 'NONE',  ( 4.195795028115014702, -4.289273350251340489, 18.50428920362019980 ) ) ;
#8366 = CARTESIAN_POINT ( 'NONE',  ( -2.500000000000000000, 0.000000000000000000, -1.399999997815050357 ) ) ;
#8367 = STYLED_ITEM ( 'NONE', ( #6540 ), #4943 ) ;
#8368 = CARTESIAN_POINT ( 'NONE',  ( -5.858813228503648496, -2.179803269293280721, 4.026227171247319880 ) ) ;
#8369 = CARTESIAN_POINT ( 'NONE',  ( 2.500000000000000444, 184.0000000000000000, 7.000000000000000000 ) ) ;
#8370 = CARTESIAN_POINT ( 'NONE',  ( -2.500000000000000000, -1.035533905932739307, 0.9499999999999999556 ) ) ;
#8371 = CARTESIAN_POINT ( 'NONE',  ( -5.558508435838198203, 2.857531096718914476, 11.49999999999998224 ) ) ;
#8372 = CARTESIAN_POINT ( 'NONE',  ( -5.842945980534674177, 1.369128644668844652, 30.12621569129737864 ) ) ;
#8373 = EDGE_LOOP ( 'NONE', ( #13675, #14920, #11994, #1292 ) ) ;
#8374 = ORIENTED_EDGE ( 'NONE', *, *, #11282, .F. ) ;
#8375 = PRESENTATION_LAYER_ASSIGNMENT (  '', '', ( #7858 ) ) ;
#8376 = ORIENTED_EDGE ( 'NONE', *, *, #14362, .T. ) ;
#8377 = CARTESIAN_POINT ( 'NONE',  ( 0.2602597315884058182, 228.9118724663684645, 8.872930549436382819 ) ) ;
#8378 = EDGE_LOOP ( 'NONE', ( #2368, #6792, #3891, #2568 ) ) ;
#8379 = EDGE_CURVE ( 'NONE', #12014, #3363, #4719, .T. ) ;
#8380 = CARTESIAN_POINT ( 'NONE',  ( 1.035533905932737531, 2.500000000000000444, -1.649999997815050579 ) ) ;
#8381 = CARTESIAN_POINT ( 'NONE',  ( -0.7993282387949094403, 5.947240459526536682, 25.11484358216957347 ) ) ;
#8382 = CARTESIAN_POINT ( 'NONE',  ( -1.035533905932737753, 2.500000000000000444, -0.05000000000000013461 ) ) ;
#8383 = CARTESIAN_POINT ( 'NONE',  ( 2.066987300000000083, 187.6999999989075150, 6.143825827087054492 ) ) ;
#8385 = CARTESIAN_POINT ( 'NONE',  ( -1.767766952966368432, -1.767766952966369320, -1.393000000021849649 ) ) ;
#8384 = B_SPLINE_CURVE_WITH_KNOTS ( 'NONE', 3,
 ( #4171, #13869, #7990, #12831, #2013, #1779, #12682, #3209, #8069, #6886, #6654, #11485, #588, #5766, #979, #13145, #4647, #4487 ),
 .UNSPECIFIED., .F., .F.,
 ( 4, 2, 2, 2, 2, 2, 2, 2, 4 ),
 ( 0.000000000000000000, 0.0003914898357794963568, 0.0007829796715589927136, 0.001174469507338489179, 0.001565959343117986511, 0.001957449178897483627, 0.002348939014676980960, 0.002740428850456478726, 0.003131918686235975625 ),
 .UNSPECIFIED. ) ;
#8386 = CARTESIAN_POINT ( 'NONE',  ( -2.066987299999999639, 0.000000000000000000, 2.050000001092474822 ) ) ;
#8387 = ITEM_DEFINED_TRANSFORMATION ( 'NONE', 'NONE', #5356,  #14201 ) ;
#8388 = CARTESIAN_POINT ( 'NONE',  ( 3.796994071234844259E-16, -2.066987299999999639, -0.9499999989075252893 ) ) ;
#8389 = ADVANCED_FACE ( 'NONE', ( #11712 ), #5680, .F. ) ;
#8390 = CARTESIAN_POINT ( 'NONE',  ( 2.817313151351187983, -5.579000502529432026, 5.000000000000004441 ) ) ;
#8391 = CARTESIAN_POINT ( 'NONE',  ( 1.240393925004889208, 226.4108590421392933, 4.739248726333301853 ) ) ;
#8392 = AXIS2_PLACEMENT_3D ( 'NONE', #8562, #1219, #3530 ) ;
#8393 = DIRECTION ( 'NONE',  ( -1.000000000000000000, 3.326610055774637112E-18, 1.062480551894331163E-17 ) ) ;
#8394 = VERTEX_POINT ( 'NONE', #2081 ) ;
#8395 = VERTEX_POINT ( 'NONE', #4562 ) ;
#8396 = DIRECTION ( 'NONE',  ( 0.8090169943749506709, -0.5877852522924689183, 0.000000000000000000 ) ) ;
#8397 = ORIENTED_EDGE ( 'NONE', *, *, #8678, .F. ) ;
#8398 = ORIENTED_EDGE ( 'NONE', *, *, #70, .T. ) ;
#8399 = CARTESIAN_POINT ( 'NONE',  ( -6.176542424588102875, -0.9554180641286524889, 30.86765874365832119 ) ) ;
#8400 = FACE_BOUND ( 'NONE', #7486, .T. ) ;
#8401 = CARTESIAN_POINT ( 'NONE',  ( 2.500000000000000000, 3.061616997868383141E-16, 2.500000000000000000 ) ) ;
#8402 = AXIS2_PLACEMENT_3D ( 'NONE', #3876, #3803, #13436 ) ;
#8403 = CARTESIAN_POINT ( 'NONE',  ( -7.180990026460683850, -3.384707322287710873, 24.49999999999999289 ) ) ;
#8404 = UNCERTAINTY_MEASURE_WITH_UNIT (LENGTH_MEASURE( 1.000000000000000082E-05 ), #775, 'distance_accuracy_value', 'NONE');
#8405 = CARTESIAN_POINT ( 'NONE',  ( 5.375913338529156427, -2.664979843780304058, 17.49571079637979665 ) ) ;
#8406 = CARTESIAN_POINT ( 'NONE',  ( -0.1323408341372861174, -6.250000000000005329, 25.50000000000000355 ) ) ;
#8407 = CARTESIAN_POINT ( 'NONE',  ( -4.291255145204106114, 4.544933371694646063, 12.11396179408069607 ) ) ;
#8408 = CARTESIAN_POINT ( 'NONE',  ( 5.935543223013850955, 0.8771126767607274610, 30.86935038651144936 ) ) ;
#8409 = CARTESIAN_POINT ( 'NONE',  ( -4.435347140101154828, -4.403429997944389385, 24.49999999999999289 ) ) ;
#8410 = CARTESIAN_POINT ( 'NONE',  ( 9.750000000000003553, 66.00000000000000000, 1.020968533498575461E-13 ) ) ;
#8411 = CARTESIAN_POINT ( 'NONE',  ( -1.767766952966369765, 186.7999999978150356, 8.767766952966368876 ) ) ;
#8412 = CARTESIAN_POINT ( 'NONE',  ( 0.6359992007181909379, 226.3469529472061765, 4.550856198837272437 ) ) ;
#8413 = PLANE ( 'NONE',  #14136 ) ;
#8414 = CARTESIAN_POINT ( 'NONE',  ( 5.903230462362950348, 1.077253041748909013, 31.61442521571937547 ) ) ;
#8415 = EDGE_LOOP ( 'NONE', ( #10052, #11065 ) ) ;
#8416 = CARTESIAN_POINT ( 'NONE',  ( -1.016439536705160407E-17, 228.2551366889529731, 10.16828399152529272 ) ) ;
#8417 = CARTESIAN_POINT ( 'NONE',  ( 0.5039079366033171192, -5.980031194523144578, 10.62637068109811800 ) ) ;
#8419 = ORIENTED_EDGE ( 'NONE', *, *, #5497, .F. ) ;
#8418 = CARTESIAN_POINT ( 'NONE',  ( 0.000000000000000000, 0.000000000000000000, 0.000000000000000000 ) ) ;
#8420 = CARTESIAN_POINT ( 'NONE',  ( 0.0002870078139504136732, -0.3999999999999958589, 2.459819222911289405 ) ) ;
#8421 = DIRECTION ( 'NONE',  ( -0.9510565162951545304, 0.3090169943749447867, 0.000000000000000000 ) ) ;
#8422 = CARTESIAN_POINT ( 'NONE',  ( 2.817313151350925526, 5.579000502529565253, 24.36939309276499799 ) ) ;
#8423 = CARTESIAN_POINT ( 'NONE',  ( 0.8561741729129463963, -2.066987299999999195, -0.6999999989075250673 ) ) ;
#8424 = CARTESIAN_POINT ( 'NONE',  ( -1.172763158762331281, 226.4018383945252992, 4.712657049679232379 ) ) ;
#8425 = CARTESIAN_POINT ( 'NONE',  ( -0.5042675786779022840, -6.230788509548840892, 31.87331068310447790 ) ) ;
#8426 = CARTESIAN_POINT ( 'NONE',  ( 2.500000000000000444, 186.2800000002184788, 8.035533905932739529 ) ) ;
#8427 = CARTESIAN_POINT ( 'NONE',  ( -2.817313151351189315, 5.579000502529432026, 5.000000000000004441 ) ) ;
#8428 = CARTESIAN_POINT ( 'NONE',  ( -0.7328022267957914337, 227.6546247107034446, 5.241927322362504249 ) ) ;
#8429 = CARTESIAN_POINT ( 'NONE',  ( -2.913793338554793166E-15, 228.9118723800512782, 8.872930300147347182 ) ) ;
#8430 = CARTESIAN_POINT ( 'NONE',  ( -2.066987299999999639, 0.8561741729129455081, -0.1999999989075250117 ) ) ;
#8431 = CARTESIAN_POINT ( 'NONE',  ( 0.8738118504725876923, 5.936246475285029689, 31.50357242174242600 ) ) ;
#8432 = ORIENTED_EDGE ( 'NONE', *, *, #6898, .F. ) ;
#8434 = CARTESIAN_POINT ( 'NONE',  ( 2.066987299999999639, 188.1999999989075150, 7.856174172912946396 ) ) ;
#8433 = PRODUCT_DEFINITION_SHAPE ( 'NONE', 'NONE',  #15082 ) ;
#8435 = AXIS2_PLACEMENT_3D ( 'NONE', #664, #11492, #1863 ) ;
#8436 = CARTESIAN_POINT ( 'NONE',  ( -2.066987300000001415, 184.6999999989075150, 7.856174172912944620 ) ) ;
#8437 = PLANE ( 'NONE',  #13146 ) ;
#8438 = ORIENTED_EDGE ( 'NONE', *, *, #12750, .F. ) ;
#8439 = EDGE_CURVE ( 'NONE', #15704, #5008, #9208, .T. ) ;
#8440 = LINE ( 'NONE', #9711, #12943 ) ;
#8441 = FACE_BOUND ( 'NONE', #11004, .T. ) ;
#8442 = DIRECTION ( 'NONE',  ( 0.000000000000000000, 0.000000000000000000, -1.000000000000000000 ) ) ;
#8443 = CARTESIAN_POINT ( 'NONE',  ( 0.9740012993920699191, 6.173846968979631811, 11.76164920628442978 ) ) ;
#8444 = CARTESIAN_POINT ( 'NONE',  ( -2.066987300000000971, 185.4999999989075263, 7.856174172912944620 ) ) ;
#8445 = CARTESIAN_POINT ( 'NONE',  ( 3.010624175977939299, -5.190832888732245465, 18.79888242247940155 ) ) ;
#8446 = AXIS2_PLACEMENT_3D ( 'NONE', #1223, #2257, #12046 ) ;
#8447 = CARTESIAN_POINT ( 'NONE',  ( -1.767766952966369098, 1.767766952966369098, -3.099999997815050090 ) ) ;
#8448 = CARTESIAN_POINT ( 'NONE',  ( 9.750000000000003553, -1.020968533498575335E-13, 2.000000000000001776 ) ) ;
#8449 = CARTESIAN_POINT ( 'NONE',  ( 5.935543223013862502, -0.8771126767606430841, 31.00000000000000000 ) ) ;
#8450 = CARTESIAN_POINT ( 'NONE',  ( 0.6139731865240156683, -6.220476368274049150, 30.19975545601932865 ) ) ;
#8451 = CARTESIAN_POINT ( 'NONE',  ( 5.409274167810623091, 2.597759609440709827, 4.384806175511482884 ) ) ;
#8452 = CARTESIAN_POINT ( 'NONE',  ( 2.782156709077223677, 5.316215864844147099, 23.99687951097623184 ) ) ;
#8453 = EDGE_CURVE ( 'NONE', #13930, #3549, #10835, .T. ) ;
#8454 = EDGE_LOOP ( 'NONE', ( #61, #241, #8480, #9898 ) ) ;
#8455 = VERTEX_POINT ( 'NONE', #8386 ) ;
#8456 = EDGE_CURVE ( 'NONE', #3287, #14081, #321, .T. ) ;
#8457 = ORIENTED_EDGE ( 'NONE', *, *, #1564, .T. ) ;
#8458 = AXIS2_PLACEMENT_3D ( 'NONE', #482, #11380, #402 ) ;
#8459 = CARTESIAN_POINT ( 'NONE',  ( -4.267992336621238891, 4.217442018459959030, 11.76194324003145120 ) ) ;
#8460 = VERTEX_POINT ( 'NONE', #172 ) ;
#8461 = PRODUCT_DEFINITION_SHAPE ( 'NONE', 'NONE',  #15763 ) ;
#8462 = CARTESIAN_POINT ( 'NONE',  ( 2.500000000000000444, -1.035533905932737309, -1.849999997815050534 ) ) ;
#8463 = PLANE ( 'NONE',  #10111 ) ;
#8464 = DIRECTION ( 'NONE',  ( 0.000000000000000000, 1.000000000000000000, 0.000000000000000000 ) ) ;
#8465 = CARTESIAN_POINT ( 'NONE',  ( 1.461580736456473018, 186.1499999989075320, 5.538419263543527649 ) ) ;
#8466 = CARTESIAN_POINT ( 'NONE',  ( -2.500000000000000444, 1.035533905932737753, 0.8500000000000001998 ) ) ;
#8467 =( BOUNDED_CURVE ( )  B_SPLINE_CURVE ( 2, ( #3051, #423, #6567, #7981, #9182, #1772, #6645, #9258, #7746 ),
 .UNSPECIFIED., .F., .F. ) 
 B_SPLINE_CURVE_WITH_KNOTS ( ( 3, 2, 2, 2, 3 ),
 ( 0.000000000000000000, 0.01785714285714285268, 0.03571428571428570536, 0.05357142857142856152, 0.07142857142857141073 ),
 .UNSPECIFIED. ) 
 CURVE ( )  GEOMETRIC_REPRESENTATION_ITEM ( )  RATIONAL_B_SPLINE_CURVE ( ( 1.000000000000000000, 0.9238795325112867385, 1.000000000000000000, 0.9238795325112867385, 1.000000000000000000, 0.9238795325112867385, 1.000000000000000000, 0.9238795325112868495, 0.9999999999999998890 ) ) 
 REPRESENTATION_ITEM ( '' )  );
#8468 = B_SPLINE_CURVE_WITH_KNOTS ( 'NONE', 3,
 ( #7121, #14339, #2169, #2252, #8313, #11957, #10773, #7201, #2329, #3367, #15630, #4734, #12117, #3606, #5846, #13237, #12042, #9582 ),
 .UNSPECIFIED., .F., .F.,
 ( 4, 2, 2, 2, 2, 2, 2, 2, 4 ),
 ( 0.000000000000000000, 0.0003914357524127469435, 0.0007828715048254938870, 0.001174307257238240993, 0.001565743009650987774, 0.001957178762063734555, 0.002348614514476480251, 0.002740050266889226815, 0.003131486019301972078 ),
 .UNSPECIFIED. ) ;
#8469 = CARTESIAN_POINT ( 'NONE',  ( -5.558508435838198203, 2.857531096718914476, 11.49999999999998224 ) ) ;
#8470 = CONTEXT_DEPENDENT_SHAPE_REPRESENTATION ( #2116, #10730 ) ;
#8471 = CARTESIAN_POINT ( 'NONE',  ( -2.066987299999999195, -0.8561741729129466183, 1.500000001092474777 ) ) ;
#8472 = AXIS2_PLACEMENT_3D ( 'NONE', #4166, #10218, #11249 ) ;
#8473 = EDGE_CURVE ( 'NONE', #1512, #7319, #95, .T. ) ;
#8474 = DIRECTION ( 'NONE',  ( -0.000000000000000000, -1.000000000000000000, -0.000000000000000000 ) ) ;
#8475 = CARTESIAN_POINT ( 'NONE',  ( -2.052299789776659722, 226.5858468330626465, 5.255005641065958244 ) ) ;
#8476 = FACE_OUTER_BOUND ( 'NONE', #4788, .T. ) ;
#8477 = ORIENTED_EDGE ( 'NONE', *, *, #12999, .F. ) ;
#8478 = VERTEX_POINT ( 'NONE', #9738 ) ;
#8479 = CARTESIAN_POINT ( 'NONE',  ( 0.000000000000000000, 0.000000000000000000, 2.500000000000000000 ) ) ;
#8480 = ORIENTED_EDGE ( 'NONE', *, *, #13705, .T. ) ;
#8481 =( BOUNDED_CURVE ( )  B_SPLINE_CURVE ( 3, ( #2933, #9292, #9145, #9449 ),
 .UNSPECIFIED., .F., .F. ) 
 B_SPLINE_CURVE_WITH_KNOTS ( ( 4, 4 ),
 ( 0.5000000000000000000, 0.5000594734819727716 ),
 .UNSPECIFIED. ) 
 CURVE ( )  GEOMETRIC_REPRESENTATION_ITEM ( )  RATIONAL_B_SPLINE_CURVE ( ( 0.9996420244238370945, 0.9997613282504840271, 0.9998806534425321857, 0.9999999999999814593 ) ) 
 REPRESENTATION_ITEM ( '' )  );
#8482 = ORIENTED_EDGE ( 'NONE', *, *, #13524, .T. ) ;
#8483 = CARTESIAN_POINT ( 'NONE',  ( -5.570820891630731353, 2.833901239560472796, 24.76236973443873524 ) ) ;
#8484 = CARTESIAN_POINT ( 'NONE',  ( 2.668367453516585108, -5.373994336898155311, 17.86935038651144225 ) ) ;
#8485 = CARTESIAN_POINT ( 'NONE',  ( 0.2619041840694849577, -6.245686665308502583, 4.026058494337955374 ) ) ;
#8486 = EDGE_CURVE ( 'NONE', #10533, #14401, #18, .T. ) ;
#8487 = CARTESIAN_POINT ( 'NONE',  ( -6.155867707731105476, -1.081837891425919462, 31.50436969680151833 ) ) ;
#8488 = CARTESIAN_POINT ( 'NONE',  ( 3.159612573729145168, -5.393342049074681732, 23.69973484982322987 ) ) ;
#8489 = CARTESIAN_POINT ( 'NONE',  ( -4.142620314836348960, -4.341347824677533218, 12.11442521571935238 ) ) ;
#8490 = CARTESIAN_POINT ( 'NONE',  ( -3.458467055437342008, 5.207305717053796634, 12.47359571723300498 ) ) ;
#8491 = ADVANCED_FACE ( 'NONE', ( #7343 ), #6076, .F. ) ;
#8492 = CARTESIAN_POINT ( 'NONE',  ( 2.500000000000000444, 184.0000000000000000, 7.000000000000000000 ) ) ;
#8493 = CARTESIAN_POINT ( 'NONE',  ( 0.7993282387953127843, -5.947240459526482503, 25.11484358216956991 ) ) ;
#8494 = DIRECTION ( 'NONE',  ( 0.000000000000000000, 1.000000000000000000, 0.000000000000000000 ) ) ;
#8495 = CARTESIAN_POINT ( 'NONE',  ( 1.767766952966369098, 188.7999999978150356, 5.232233047033630235 ) ) ;
#8496 = CARTESIAN_POINT ( 'NONE',  ( 1.628454131612142364, 226.4793820939146372, 4.941229787183066158 ) ) ;
#8497 = CARTESIAN_POINT ( 'NONE',  ( -5.615973259022252861, -2.743340227996308389, 18.50389213124969956 ) ) ;
#8498 = CARTESIAN_POINT ( 'NONE',  ( 0.08612929575471790777, 189.4418673012125680, 3.980892606666732281 ) ) ;
#8499 = EDGE_LOOP ( 'NONE', ( #11376, #337 ) ) ;
#8500 = DIRECTION ( 'NONE',  ( 0.000000000000000000, 0.000000000000000000, -1.000000000000000000 ) ) ;
#8501 = CARTESIAN_POINT ( 'NONE',  ( 0.2619456584322786274, -5.995505046955611483, 10.52607193928646367 ) ) ;
#8503 = ORIENTED_EDGE ( 'NONE', *, *, #14362, .F. ) ;
#8502 = CARTESIAN_POINT ( 'NONE',  ( 13.50000000000000000, 2.000000000000000000, -8.673617379884035472E-16 ) ) ;
#8504 = CARTESIAN_POINT ( 'NONE',  ( 0.0008577403172727038339, -0.3999999999999958589, 2.464205331206099192 ) ) ;
#8505 = CYLINDRICAL_SURFACE ( 'NONE', #3837, 2.500000000000000000 ) ;
#8506 = CARTESIAN_POINT ( 'NONE',  ( -4.286401442266640771, 4.198423832313082471, 11.49999999999998224 ) ) ;
#8507 = CARTESIAN_POINT ( 'NONE',  ( -0.8561741729129458411, -2.066987299999999195, 1.600000001092474866 ) ) ;
#8508 = CARTESIAN_POINT ( 'NONE',  ( -3.567258970016137010, 5.133675764669563435, 23.49991780678443121 ) ) ;
#8509 =( NAMED_UNIT ( * ) PLANE_ANGLE_UNIT ( ) SI_UNIT ( $, .RADIAN. ) );
#8510 = CARTESIAN_POINT ( 'NONE',  ( -6.142844459177239536, 1.156093792145192145, 12.11560192892920895 ) ) ;
#8511 = CARTESIAN_POINT ( 'NONE',  ( 2.500000000000000444, 184.0000000000000000, 7.000000000000000000 ) ) ;
#8512 = CARTESIAN_POINT ( 'NONE',  ( 1.984153134209927671, 228.3142122347729526, 7.146853712282291049 ) ) ;
#8513 = CARTESIAN_POINT ( 'NONE',  ( 0.8561741729129452860, 2.066987299999999639, 1.200000001092474733 ) ) ;
#8514 = CARTESIAN_POINT ( 'NONE',  ( 6.020822430078810683, 1.681351817312345842, 17.02591457665827690 ) ) ;
#8515 = B_SPLINE_CURVE_WITH_KNOTS ( 'NONE', 3,
 ( #6395, #11228, #5191, #11927, #10509, #12962 ),
 .UNSPECIFIED., .F., .F.,
 ( 4, 2, 4 ),
 ( 0.09236347834653250988, 0.5261283886372931651, 0.9760345799090694996 ),
 .UNSPECIFIED. ) ;
#8516 = ORIENTED_EDGE ( 'NONE', *, *, #9736, .T. ) ;
#8517 = CARTESIAN_POINT ( 'NONE',  ( 2.066987300000000083, 189.0499999989075093, 7.000000000000000000 ) ) ;
#8518 = CARTESIAN_POINT ( 'NONE',  ( 0.8561741729129461742, 185.6999999989075434, 9.066987300000000971 ) ) ;
#8519 = DIRECTION ( 'NONE',  ( 0.9510565162951500895, 0.3090169943749582204, 0.000000000000000000 ) ) ;
#8520 = VERTEX_POINT ( 'NONE', #8469 ) ;
#8521 = SURFACE_STYLE_USAGE ( .BOTH. , #10970 ) ;
#8522 = CIRCLE ( 'NONE', #1637, 1.500000000000000000 ) ;
#8523 = EDGE_CURVE ( 'NONE', #14489, #3268, #14310, .T. ) ;
#8524 = CARTESIAN_POINT ( 'NONE',  ( 2.500000000000000000, 3.061616997868383141E-16, 2.500000000000000000 ) ) ;
#8525 = LINE ( 'NONE', #10814, #4414 ) ;
#8526 = LINE ( 'NONE', #12239, #8857 ) ;
#8527 = CARTESIAN_POINT ( 'NONE',  ( -2.066987300000000971, 188.5999999989074922, 6.143825827087054492 ) ) ;
#8528 = CARTESIAN_POINT ( 'NONE',  ( 3.106366801611956330, -5.134708448381311463, 18.87303779027049799 ) ) ;
#8529 = CARTESIAN_POINT ( 'NONE',  ( -1.035533905932738197, -2.500000000000000000, -2.849999997815050978 ) ) ;
#8530 = CARTESIAN_POINT ( 'NONE',  ( 1.354942164306246880E-13, -6.000000000000000888, 16.99999999999998579 ) ) ;
#8531 = PLANE ( 'NONE',  #6707 ) ;
#8532 = CARTESIAN_POINT ( 'NONE',  ( -3.159082487394813565, 5.393634094348312757, 30.20045537531155944 ) ) ;
#8533 = CARTESIAN_POINT ( 'NONE',  ( 5.665824935993584610, 1.978765057080994483, 4.000049463537776795 ) ) ;
#8534 = CARTESIAN_POINT ( 'NONE',  ( 2.500000000000000444, 187.2000000000000171, 7.000000000000000000 ) ) ;
#8535 = ADVANCED_FACE ( 'NONE', ( #2317 ), #14284, .T. ) ;
#8536 = ORIENTED_EDGE ( 'NONE', *, *, #5963, .F. ) ;
#8537 = EDGE_LOOP ( 'NONE', ( #15687, #6047 ) ) ;
#8538 = VERTEX_POINT ( 'NONE', #11073 ) ;
#8539 = CARTESIAN_POINT ( 'NONE',  ( -3.011139120916709988, 5.190534000030228690, 25.29931806258175087 ) ) ;
#8540 = EDGE_LOOP ( 'NONE', ( #8557, #13620, #7989, #7427, #10674 ) ) ;
#8541 = CARTESIAN_POINT ( 'NONE',  ( 2.500000000000000444, -1.035533905932737309, -2.649999997815050357 ) ) ;
#8542 = B_SPLINE_CURVE_WITH_KNOTS ( 'NONE', 3,
 ( #6905, #13007, #15330, #14045, #1873, #15171, #5552, #6748, #11581, #678, #11662, #6827, #15407, #15249, #4504, #10399, #6979, #3154 ),
 .UNSPECIFIED., .F., .F.,
 ( 4, 2, 2, 2, 2, 2, 2, 2, 4 ),
 ( 0.003131490185285879316, 0.003522829482338505399, 0.003914168779391132350, 0.004305508076443757999, 0.004696847373496385383, 0.005088186670549011033, 0.005479525967601636682, 0.005870865264654263199, 0.006262204561706889716 ),
 .UNSPECIFIED. ) ;
#8543 = AXIS2_PLACEMENT_3D ( 'NONE', #15254, #3081, #6986 ) ;
#8544 = FACE_BOUND ( 'NONE', #7179, .T. ) ;
#8545 = AXIS2_PLACEMENT_3D ( 'NONE', #14722, #3810, #1416 ) ;
#8546 = CARTESIAN_POINT ( 'NONE',  ( 2.500000000000000000, 3.061616997868383141E-16, -0.2999999999999999334 ) ) ;
#8547 = CARTESIAN_POINT ( 'NONE',  ( -2.066987300000000971, 187.9999999989075263, 6.143825827087054492 ) ) ;
#8548 = CARTESIAN_POINT ( 'NONE',  ( 2.500000000000000444, -1.035533905932737309, 2.049999999999999822 ) ) ;
#8549 = CARTESIAN_POINT ( 'NONE',  ( -5.746996058422787712, 1.729015645941882839, 32.00007961174476634 ) ) ;
#8550 = EDGE_CURVE ( 'NONE', #12174, #15156, #12266, .T. ) ;
#8551 = CONTEXT_DEPENDENT_SHAPE_REPRESENTATION ( #11578, #13131 ) ;
#8552 = CARTESIAN_POINT ( 'NONE',  ( -5.903843691985159126, -2.055287728870867525, 25.50004906876533184 ) ) ;
#8553 = CARTESIAN_POINT ( 'NONE',  ( -0.8561741729129455081, 2.066987299999999639, 2.100000001092475088 ) ) ;
#8554 = CARTESIAN_POINT ( 'NONE',  ( -1.035533905932737753, 2.500000000000000444, -2.450000000000000178 ) ) ;
#8555 = CARTESIAN_POINT ( 'NONE',  ( -2.087773716237738331, 226.5967140655768048, 5.287030890998575927 ) ) ;
#8556 = CARTESIAN_POINT ( 'NONE',  ( 0.000000000000000000, 0.000000000000000000, 2.500000000000000000 ) ) ;
#8557 = ORIENTED_EDGE ( 'NONE', *, *, #2877, .F. ) ;
#8558 = ORIENTED_EDGE ( 'NONE', *, *, #2240, .F. ) ;
#8559 = VERTEX_POINT ( 'NONE', #7495 ) ;
#8560 = ORIENTED_EDGE ( 'NONE', *, *, #11808, .T. ) ;
#8561 = CARTESIAN_POINT ( 'NONE',  ( -6.020865209844592059, -1.681180471732148130, 30.02599901976670438 ) ) ;
#8562 = CARTESIAN_POINT ( 'NONE',  ( -1.084202172485504434E-15, -3.464101615137755275, -5.500000000000000000 ) ) ;
#8563 = FACE_OUTER_BOUND ( 'NONE', #11587, .T. ) ;
#8564 = CARTESIAN_POINT ( 'NONE',  ( -5.770167736194690811, -2.404664418229182754, 31.87367328635992081 ) ) ;
#8565 = UNCERTAINTY_MEASURE_WITH_UNIT (LENGTH_MEASURE( 1.000000000000000082E-05 ), #15417, 'distance_accuracy_value', 'NONE');
#8566 = FACE_OUTER_BOUND ( 'NONE', #8028, .T. ) ;
#8567 = CARTESIAN_POINT ( 'NONE',  ( -2.782769401326190106, -5.315896561274842114, 12.00428920362018914 ) ) ;
#8568 = CARTESIAN_POINT ( 'NONE',  ( 0.000000000000000000, 2.000000000000000000, 0.000000000000000000 ) ) ;
#8569 = CARTESIAN_POINT ( 'NONE',  ( 5.665824935993590827, 1.978765057080975387, 30.00004946353777413 ) ) ;
#8570 = CARTESIAN_POINT ( 'NONE',  ( 1.767766952966369098, 188.0999999999999943, 5.232233047033630235 ) ) ;
#8571 = DIRECTION ( 'NONE',  ( 0.000000000000000000, 1.000000000000000000, 0.000000000000000000 ) ) ;
#8572 = CARTESIAN_POINT ( 'NONE',  ( -6.844026213814746740E-16, 187.6999999978150697, 9.500000000000001776 ) ) ;
#8573 = CARTESIAN_POINT ( 'NONE',  ( 2.998835045281009304, 227.2583357984985639, 7.235791215503737384 ) ) ;
#8574 = CARTESIAN_POINT ( 'NONE',  ( -5.935543223013847403, -0.8771126767607489993, 5.000000000000004441 ) ) ;
#8575 = ADVANCED_FACE ( 'NONE', ( #2643 ), #3828, .F. ) ;
#8576 = CARTESIAN_POINT ( 'NONE',  ( -1.726536558038261449, 188.9999999997880877, 8.813927586020868787 ) ) ;
#8577 = EDGE_LOOP ( 'NONE', ( #3568, #6501, #9082, #10983 ) ) ;
#8578 = CARTESIAN_POINT ( 'NONE',  ( -5.531209434046333584, 2.328189801702630124, 12.37303779027049089 ) ) ;
#8579 = VECTOR ( 'NONE', #2457, 1000.000000000000000 ) ;
#8580 = CARTESIAN_POINT ( 'NONE',  ( 0.000000000000000000, 0.000000000000000000, 2.500000000000000000 ) ) ;
#8581 = CARTESIAN_POINT ( 'NONE',  ( 2.500000000000000444, 1.035533905932737975, -1.050000000000000044 ) ) ;
#8582 = CARTESIAN_POINT ( 'NONE',  ( 6.000000000000000000, 7.347880794884118750E-16, 52.97056274847714263 ) ) ;
#8583 = CARTESIAN_POINT ( 'NONE',  ( 1.034563906089895458, 226.3842683607827553, 4.660856843270724248 ) ) ;
#8584 = CYLINDRICAL_SURFACE ( 'NONE', #8959, 1.000000000000000222 ) ;
#8585 = CARTESIAN_POINT ( 'NONE',  ( 0.8561741729129451750, 2.066987299999999639, 0.4000000010924749105 ) ) ;
#8586 = CARTESIAN_POINT ( 'NONE',  ( -2.897581130414634077E-17, 22.00000000000000000, -9.750000000000003553 ) ) ;
#8587 = CARTESIAN_POINT ( 'NONE',  ( -6.155854678529477653, 1.081900940642092523, 12.00425949503009626 ) ) ;
#8588 = CARTESIAN_POINT ( 'NONE',  ( -1.035533905932739751, 187.6800000002184845, 9.500000000000003553 ) ) ;
#8589 = FACE_BOUND ( 'NONE', #8077, .T. ) ;
#8590 = VECTOR ( 'NONE', #13022, 1000.000000000000000 ) ;
#8591 = CARTESIAN_POINT ( 'NONE',  ( 1.864425960470169619, 228.0311117417621745, 6.329243341474429130 ) ) ;
#8592 = CARTESIAN_POINT ( 'NONE',  ( -2.066987299999999195, -0.8561741729129467293, 0.7000000010924749549 ) ) ;
#8593 = EDGE_CURVE ( 'NONE', #8910, #2429, #11502, .T. ) ;
#8594 = CARTESIAN_POINT ( 'NONE',  ( -1.530808498934191571E-16, 2.500000000000000000, 1.500000000000000000 ) ) ;
#8595 = ORIENTED_EDGE ( 'NONE', *, *, #5524, .F. ) ;
#8596 = CARTESIAN_POINT ( 'NONE',  ( -0.8561741729129471734, 187.1999999989075434, 9.066987300000000971 ) ) ;
#8597 = CARTESIAN_POINT ( 'NONE',  ( 2.066987300000000971, 185.0999999989074922, 6.143825827087054492 ) ) ;
#8598 = CARTESIAN_POINT ( 'NONE',  ( 5.317509234264026219, 2.779225709350867213, 24.36760611998364823 ) ) ;
#8599 =( GEOMETRIC_REPRESENTATION_CONTEXT ( 3 ) GLOBAL_UNCERTAINTY_ASSIGNED_CONTEXT ( ( #13885 ) ) GLOBAL_UNIT_ASSIGNED_CONTEXT ( ( #13790, #4005, #5297 ) ) REPRESENTATION_CONTEXT ( 'NONE', 'WORKASPACE' ) );
#8601 = ORIENTED_EDGE ( 'NONE', *, *, #10094, .F. ) ;
#8600 = CARTESIAN_POINT ( 'NONE',  ( -2.066987300000000527, 185.6999999989075150, 7.856174172912944620 ) ) ;
#8602 = CARTESIAN_POINT ( 'NONE',  ( 2.030576276931546336E-13, -6.250000000000000888, 24.49999999999999289 ) ) ;
#8603 = CIRCLE ( 'NONE', #6303, 3.118365096457674124 ) ;
#8604 = CARTESIAN_POINT ( 'NONE',  ( 5.915699123067165388, -1.003533581835512223, 5.503897950159859498 ) ) ;
#8605 = CARTESIAN_POINT ( 'NONE',  ( 0.000000000000000000, 201.6409668649146738, 13.30942870683726298 ) ) ;
#8606 = CARTESIAN_POINT ( 'NONE',  ( 2.066987299999999639, 188.9999999989075263, 7.856174172912946396 ) ) ;
#8607 = CARTESIAN_POINT ( 'NONE',  ( 5.843075991566629490, -1.368655265450851033, 25.37364704684422634 ) ) ;
#8608 = CARTESIAN_POINT ( 'NONE',  ( 0.6765616680526839177, 189.0525113742165502, 10.11220174261750593 ) ) ;
#8609 = CARTESIAN_POINT ( 'NONE',  ( 0.000000000000000000, 184.0000000000000000, 0.000000000000000000 ) ) ;
#8610 = LINE ( 'NONE', #4864, #10758 ) ;
#8611 = CARTESIAN_POINT ( 'NONE',  ( -5.866984344570847831, 1.259800266528558810, 10.70068193741824736 ) ) ;
#8612 = DIRECTION ( 'NONE',  ( 0.000000000000000000, 0.000000000000000000, 1.000000000000000000 ) ) ;
#8613 = CARTESIAN_POINT ( 'NONE',  ( -5.487348639458900834, 2.428538342494392488, 30.19977782616121331 ) ) ;
#8614 = EDGE_LOOP ( 'NONE', ( #722, #7349 ) ) ;
#8615 = ORIENTED_EDGE ( 'NONE', *, *, #13288, .F. ) ;
#8616 = VERTEX_POINT ( 'NONE', #5993 ) ;
#8617 = DIRECTION ( 'NONE',  ( 0.000000000000000000, -1.000000000000000000, 0.000000000000000000 ) ) ;
#8618 = ORIENTED_EDGE ( 'NONE', *, *, #4720, .T. ) ;
#8619 = AXIS2_PLACEMENT_3D ( 'NONE', #9123, #12684, #3140 ) ;
#8620 = CARTESIAN_POINT ( 'NONE',  ( -2.066987299999999195, -0.8561741729129466183, -0.2999999989075253226 ) ) ;
#8621 = CARTESIAN_POINT ( 'NONE',  ( -5.984595133899149211, -1.806709459528761164, 12.49995078984291830 ) ) ;
#8622 = CARTESIAN_POINT ( 'NONE',  ( -1.767766952966369098, 1.767766952966369098, 0.000000000000000000 ) ) ;
#8623 = CARTESIAN_POINT ( 'NONE',  ( -1.461580736456473018, 186.3499999989075206, 5.538419263543527649 ) ) ;
#8624 = CARTESIAN_POINT ( 'NONE',  ( 2.500000000000000444, 1.035533905932737975, 0.5499999999999999334 ) ) ;
#8625 = CARTESIAN_POINT ( 'NONE',  ( -5.915641100987835799, 1.003868594704728556, 31.50428920362020335 ) ) ;
#8626 = ITEM_DEFINED_TRANSFORMATION ( 'NONE', 'NONE', #12953,  #14201 ) ;
#8627 = CARTESIAN_POINT ( 'NONE',  ( 3.311576095066635972, -5.004818610361267517, 31.97377823943292086 ) ) ;
#8628 = CARTESIAN_POINT ( 'NONE',  ( -1.461580736456472795, 1.461580736456472795, -1.249999998907525223 ) ) ;
#8629 = DIRECTION ( 'NONE',  ( 0.8090169943749506709, -0.5877852522924686962, 0.000000000000000000 ) ) ;
#8630 = CARTESIAN_POINT ( 'NONE',  ( -2.521794825564176890, 226.7667903661470348, 5.788166807254388146 ) ) ;
#8631 = APPLICATION_CONTEXT ( 'automotive_design' ) ;
#8632 = EDGE_LOOP ( 'NONE', ( #11123, #10421, #2884, #2605 ) ) ;
#8633 = AXIS2_PLACEMENT_3D ( 'NONE', #15160, #4575, #7914 ) ;
#8634 = AXIS2_PLACEMENT_3D ( 'NONE', #5577, #5651, #787 ) ;
#8635 = EDGE_LOOP ( 'NONE', ( #85, #1935, #7641, #1085 ) ) ;
#8636 = VERTEX_POINT ( 'NONE', #15698 ) ;
#8637 = CARTESIAN_POINT ( 'NONE',  ( -5.615811513734976224, -2.743665920700520733, 10.99691356133951992 ) ) ;
#8638 = CARTESIAN_POINT ( 'NONE',  ( 4.069800786343786392, 4.744882212776837527, 4.126180359549290522 ) ) ;
#8639 = EDGE_CURVE ( 'NONE', #14280, #1820, #14954, .T. ) ;
#8640 = CARTESIAN_POINT ( 'NONE',  ( 0.9740012993920164064, 6.173846968979639804, 5.261649206284398694 ) ) ;
#8641 = ADVANCED_FACE ( 'NONE', ( #14894 ), #2957, .F. ) ;
#8642 = CARTESIAN_POINT ( 'NONE',  ( -5.615973259022300823, -2.743340227996212910, 31.50389213124968890 ) ) ;
#8643 = DIRECTION ( 'NONE',  ( 6.123233995738439900E-17, 0.000000000000000000, -1.000000000000000000 ) ) ;
#8644 = CIRCLE ( 'NONE', #491, 1.499999999999999556 ) ;
#8645 = CARTESIAN_POINT ( 'NONE',  ( 2.000000000000001776, -4.163336342344337027E-16, 1.500000000000001776 ) ) ;
#8646 = CARTESIAN_POINT ( 'NONE',  ( 2.030576276931546336E-13, -6.250000000000000888, 24.49999999999999289 ) ) ;
#8647 = CARTESIAN_POINT ( 'NONE',  ( 4.000000000000001776, 184.0000000000000000, 7.000000000000000000 ) ) ;
#8648 = CARTESIAN_POINT ( 'NONE',  ( -2.500000000000000000, 0.000000000000000000, 2.500000000000000000 ) ) ;
#8649 = DIRECTION ( 'NONE',  ( 0.000000000000000000, 1.000000000000000000, 0.000000000000000000 ) ) ;
#8650 = CARTESIAN_POINT ( 'NONE',  ( 2.500000000000000000, 189.4499999978150697, 8.035533905932739529 ) ) ;
#8651 = CARTESIAN_POINT ( 'NONE',  ( 2.998712701283978710, 227.3219367242041926, 7.423021690895281743 ) ) ;
#8652 = CARTESIAN_POINT ( 'NONE',  ( -0.3319738467526104908, 189.0000000000805187, 9.481785014843145731 ) ) ;
#8653 =( GEOMETRIC_REPRESENTATION_CONTEXT ( 3 ) GLOBAL_UNCERTAINTY_ASSIGNED_CONTEXT ( ( #110 ) ) GLOBAL_UNIT_ASSIGNED_CONTEXT ( ( #6665, #11575, #1558 ) ) REPRESENTATION_CONTEXT ( 'NONE', 'WORKASPACE' ) );
#8654 = ORIENTED_EDGE ( 'NONE', *, *, #12700, .F. ) ;
#8655 = DIRECTION ( 'NONE',  ( -1.000000000000000000, 0.000000000000000000, 0.000000000000000000 ) ) ;
#8656 = CARTESIAN_POINT ( 'NONE',  ( -5.903843691985187547, 2.055287728870776487, 23.49995093123466461 ) ) ;
#8657 = CARTESIAN_POINT ( 'NONE',  ( 0.000000000000000000, 184.0000000000000000, 0.000000000000000000 ) ) ;
#8658 = CARTESIAN_POINT ( 'NONE',  ( 2.500000000000000000, 3.061616997868383141E-16, 1.300000000000000044 ) ) ;
#8659 = DIRECTION ( 'NONE',  ( 0.000000000000000000, 0.000000000000000000, -1.000000000000000000 ) ) ;
#8660 = CARTESIAN_POINT ( 'NONE',  ( 7.347880431581855163E-16, -6.250000000000000888, 4.000000000000004441 ) ) ;
#8661 = CARTESIAN_POINT ( 'NONE',  ( -2.066987299999999195, -0.8561741729129466183, 1.500000001092474777 ) ) ;
#8662 = DIRECTION ( 'NONE',  ( 0.000000000000000000, 0.000000000000000000, 1.000000000000000000 ) ) ;
#8663 = LINE ( 'NONE', #9927, #13821 ) ;
#8664 = CARTESIAN_POINT ( 'NONE',  ( -7.352245982167326943E-16, 188.5300000002185072, 9.500000000000001776 ) ) ;
#8665 = CARTESIAN_POINT ( 'NONE',  ( -1.767766952966368432, -1.767766952966369320, -0.6000000000000003109 ) ) ;
#8666 = CARTESIAN_POINT ( 'NONE',  ( 1.964981070171530675, 228.3669111765908895, 7.299051262003229290 ) ) ;
#8667 = FACE_OUTER_BOUND ( 'NONE', #9787, .T. ) ;
#8668 = CARTESIAN_POINT ( 'NONE',  ( 6.155912734541138853, 1.081577393120855435, 17.49610786875029689 ) ) ;
#8669 = ORIENTED_EDGE ( 'NONE', *, *, #5743, .F. ) ;
#8670 = DIRECTION ( 'NONE',  ( 0.000000000000000000, 0.000000000000000000, 1.000000000000000000 ) ) ;
#8671 = B_SPLINE_CURVE_WITH_KNOTS ( 'NONE', 3,
 ( #6050, #15595, #7394, #1975, #9547, #14384, #4936, #3490, #4857, #14550, #8360, #13198, #3725, #12236, #8604, #13660, #4038, #5165 ),
 .UNSPECIFIED., .F., .F.,
 ( 4, 2, 2, 2, 2, 2, 2, 2, 4 ),
 ( 0.000000000000000000, 0.0003914898357794944052, 0.0007829796715589888104, 0.001174469507338483324, 0.001565959343117977621, 0.001957449178897471918, 0.002348939014676966648, 0.002740428850456460945, 0.003131918686235955242 ),
 .UNSPECIFIED. ) ;
#8672 = CARTESIAN_POINT ( 'NONE',  ( -2.066987300000000527, 185.4499999989075150, 7.000000000000000000 ) ) ;
#8673 = CARTESIAN_POINT ( 'NONE',  ( -3.567258970015958486, -5.133675764669688668, 12.50008219321555103 ) ) ;
#8675 = VERTEX_POINT ( 'NONE', #4066 ) ;
#8674 = CARTESIAN_POINT ( 'NONE',  ( -4.946672411965113980E-16, 185.8499999989075206, 9.066987300000000971 ) ) ;
#8676 = CARTESIAN_POINT ( 'NONE',  ( -2.500000000000000444, 184.4000000000000057, 7.000000000000000000 ) ) ;
#8677 = DIRECTION ( 'NONE',  ( 0.000000000000000000, 0.000000000000000000, 1.000000000000000000 ) ) ;
#8678 = EDGE_CURVE ( 'NONE', #1133, #13435, #1847, .T. ) ;
#8679 =( LENGTH_UNIT ( ) NAMED_UNIT ( * ) SI_UNIT ( .MILLI., .METRE. ) );
#8680 = CYLINDRICAL_SURFACE ( 'NONE', #10628, 1.000000000000000666 ) ;
#8681 = CARTESIAN_POINT ( 'NONE',  ( -2.127985206219880077, 189.0000000000000000, 5.658978462642562768 ) ) ;
#8682 = PLANE ( 'NONE',  #1080 ) ;
#8683 = CARTESIAN_POINT ( 'NONE',  ( 1.767766952966369320, -1.767766952966368654, -1.899999997815050357 ) ) ;
#8684 = CARTESIAN_POINT ( 'NONE',  ( -0.1323602877611954887, -6.000000000000003553, 32.00000000000000711 ) ) ;
#8685 = EDGE_CURVE ( 'NONE', #2943, #10964, #13032, .T. ) ;
#8686 = CARTESIAN_POINT ( 'NONE',  ( 5.903230462362974329, -1.077253041748779783, 10.88557478428060676 ) ) ;
#8687 = CARTESIAN_POINT ( 'NONE',  ( -1.035533905932737753, 2.500000000000000444, -2.349999997815050090 ) ) ;
#8688 = CARTESIAN_POINT ( 'NONE',  ( -5.915653884842693166, -1.003805156977521040, 12.00439760644213294 ) ) ;
#8689 = CARTESIAN_POINT ( 'NONE',  ( -5.935543223013858949, 0.8771126767606857166, 31.00000000000000000 ) ) ;
#8690 = ORIENTED_EDGE ( 'NONE', *, *, #9440, .T. ) ;
#8691 = CARTESIAN_POINT ( 'NONE',  ( -0.8561741729129467293, 185.7999999989075093, 9.066987299999999195 ) ) ;
#8692 = ORIENTED_EDGE ( 'NONE', *, *, #6898, .T. ) ;
#8693 = EDGE_LOOP ( 'NONE', ( #11202, #11408, #11542, #3263 ) ) ;
#8694 = CARTESIAN_POINT ( 'NONE',  ( 0.000000000000000000, 184.0000000000000000, 7.000000000000000000 ) ) ;
#8695 = EDGE_LOOP ( 'NONE', ( #11890, #10694, #12913, #3640 ) ) ;
#8696 = CARTESIAN_POINT ( 'NONE',  ( 1.461580736456472573, 1.461580736456472795, -1.449999998907525178 ) ) ;
#8697 = CARTESIAN_POINT ( 'NONE',  ( -5.903843691985196429, -2.055287728870748065, 12.50004906876531052 ) ) ;
#8698 = CARTESIAN_POINT ( 'NONE',  ( 5.859155363331372435, 2.178872204145008151, 31.97400098023329917 ) ) ;
#8699 = CARTESIAN_POINT ( 'NONE',  ( 0.000000000000000000, 22.00000000000000000, 0.000000000000000000 ) ) ;
#8700 = CARTESIAN_POINT ( 'NONE',  ( -1.035533905932737753, 2.500000000000000444, 0.7500000000000001110 ) ) ;
#8701 = DIRECTION ( 'NONE',  ( 0.000000000000000000, 0.000000000000000000, 1.000000000000000000 ) ) ;
#8702 = CARTESIAN_POINT ( 'NONE',  ( 3.922396193919089669, -4.541970110199406108, 31.87380682714711355 ) ) ;
#8703 = CARTESIAN_POINT ( 'NONE',  ( 0.8561741729129451750, 2.066987299999999639, -2.199999998907525622 ) ) ;
#8704 = CARTESIAN_POINT ( 'NONE',  ( 6.143020266950992792, -1.155160780047631786, 10.88558052754513206 ) ) ;
#8705 = CARTESIAN_POINT ( 'NONE',  ( -2.884911204282110120, 227.0244024278241000, 6.546979792117293862 ) ) ;
#8706 = ORIENTED_EDGE ( 'NONE', *, *, #7371, .F. ) ;
#8707 = VECTOR ( 'NONE', #5931, 1000.000000000000000 ) ;
#8708 = ORIENTED_EDGE ( 'NONE', *, *, #3135, .F. ) ;
#8709 = B_SPLINE_CURVE_WITH_KNOTS ( 'NONE', 3,
 ( #12124, #3298, #3613, #9511, #14264, #14192, #12996, #8490, #9588, #2420, #14432, #2100, #3536, #8407, #10699, #13242, #14345, #2258 ),
 .UNSPECIFIED., .F., .F.,
 ( 4, 2, 2, 2, 2, 2, 2, 2, 4 ),
 ( 0.000000000000000000, 0.0003914357524127503587, 0.0007828715048255007174, 0.001174307257238250968, 0.001565743009651001435, 0.001957178762063751468, 0.002348614514476503237, 0.002740050266889254571, 0.003131486019302005472 ),
 .UNSPECIFIED. ) ;
#8710 = ORIENTED_EDGE ( 'NONE', *, *, #13716, .F. ) ;
#8711 = CARTESIAN_POINT ( 'NONE',  ( 5.621197618055712830, -2.101623592078419644, 30.02601979877761451 ) ) ;
#8712 = DIRECTION ( 'NONE',  ( 1.000000000000000000, 0.000000000000000000, 0.000000000000000000 ) ) ;
#8713 = CARTESIAN_POINT ( 'NONE',  ( 0.9737725088282187524, 6.173885267451822756, 4.737357587265641712 ) ) ;
#8714 = CARTESIAN_POINT ( 'NONE',  ( -4.286401442266628337, -4.198423832313095794, 17.99999999999998934 ) ) ;
#8715 = CARTESIAN_POINT ( 'NONE',  ( 5.940390500375550609, 6.474944468551622201, 5.000000000000004441 ) ) ;
#8716 = CARTESIAN_POINT ( 'NONE',  ( -2.500000000000000444, 186.7499999978150242, 8.035533905932737753 ) ) ;
#8717 = AXIS2_PLACEMENT_3D ( 'NONE', #9775, #14620, #8662 ) ;
#8718 = CARTESIAN_POINT ( 'NONE',  ( 5.746619684944299422, -1.730157667110755026, 12.50004932073310471 ) ) ;
#8719 = DIRECTION ( 'NONE',  ( 0.9510565162951500895, 0.3090169943749582204, 0.000000000000000000 ) ) ;
#8720 = CARTESIAN_POINT ( 'NONE',  ( 0.000000000000000000, 182.0000000000000000, 0.000000000000000000 ) ) ;
#8721 = CARTESIAN_POINT ( 'NONE',  ( 1.035533905932737975, 184.9199999975965909, 4.500000000000000888 ) ) ;
#8722 = CARTESIAN_POINT ( 'NONE',  ( -1.238081232355301875, 227.7501834494555055, 5.517906410191214306 ) ) ;
#8723 = CARTESIAN_POINT ( 'NONE',  ( 2.900052503084635358, 227.0405808247315917, 6.594625917879634258 ) ) ;
#8724 = B_SPLINE_CURVE_WITH_KNOTS ( 'NONE', 3,
 ( #9509, #9429, #6678, #9586, #3372, #12045, #1144, #14343, #13895, #905, #5773, #3008, #7866, #14430, #3533, #11510, #14262, #13156 ),
 .UNSPECIFIED., .F., .F.,
 ( 4, 2, 2, 2, 2, 2, 2, 2, 4 ),
 ( 0.000000000000000000, 0.0003914898357794975494, 0.0007829796715589950988, 0.001174469507338492648, 0.001565959343117990198, 0.001957449178897487964, 0.002348939014676985296, 0.002740428850456482629, 0.003131918686235980395 ),
 .UNSPECIFIED. ) ;
#8725 = ADVANCED_FACE ( 'NONE', ( #10045 ), #11383, .F. ) ;
#8726 = CARTESIAN_POINT ( 'NONE',  ( -0.2790400018234628354, 2.500000000000000444, -2.501110090150877152 ) ) ;
#8727 = ORIENTED_EDGE ( 'NONE', *, *, #10599, .T. ) ;
#8728 = CARTESIAN_POINT ( 'NONE',  ( -6.081464507797620378, 1.446657058464248857, 17.12619944752603729 ) ) ;
#8729 = CARTESIAN_POINT ( 'NONE',  ( 8.572527594031473190E-16, 22.00000000000000000, 7.000000000000000000 ) ) ;
#8730 = CARTESIAN_POINT ( 'NONE',  ( -4.142620314836507056, 4.341347824677379563, 23.88557478428061387 ) ) ;
#8731 = CARTESIAN_POINT ( 'NONE',  ( 5.725930890718287536, 2.506952462184140362, 30.20066851092423832 ) ) ;
#8732 = CARTESIAN_POINT ( 'NONE',  ( 2.734553966056355812, 226.8926218724402020, 6.158846296097578055 ) ) ;
#8733 = CARTESIAN_POINT ( 'NONE',  ( 2.930600586412791309, 5.520563544161844582, 23.99691356133952524 ) ) ;
#8734 = CARTESIAN_POINT ( 'NONE',  ( -2.500000000000000000, 0.000000000000000000, 1.700000000000000178 ) ) ;
#8735 = CARTESIAN_POINT ( 'NONE',  ( 5.903230462362961894, -1.077253041748847062, 4.385574784280630745 ) ) ;
#8736 =( LENGTH_UNIT ( ) NAMED_UNIT ( * ) SI_UNIT ( .MILLI., .METRE. ) );
#8737 = DIRECTION ( 'NONE',  ( -0.000000000000000000, 1.000000000000000000, -0.000000000000000000 ) ) ;
#8738 = CARTESIAN_POINT ( 'NONE',  ( -1.767766952966369542, 184.5000000000000000, 8.767766952966368876 ) ) ;
#8739 = CARTESIAN_POINT ( 'NONE',  ( 1.035533905932739085, -2.500000000000000000, -0.4499999999999999556 ) ) ;
#8740 = EDGE_CURVE ( 'NONE', #2306, #5609, #1276, .T. ) ;
#8741 = CARTESIAN_POINT ( 'NONE',  ( 1.974798917232459150, 228.1755836975312945, 6.746486589875083872 ) ) ;
#8742 = DIRECTION ( 'NONE',  ( 6.123233995736766036E-17, -1.000000000000000000, -0.000000000000000000 ) ) ;
#8743 = CARTESIAN_POINT ( 'NONE',  ( -2.841041022017357420, -5.567186575787277825, 11.23774718278287921 ) ) ;
#8744 = CARTESIAN_POINT ( 'NONE',  ( 2.066987300000000083, -0.8561741729129450640, 0.8000000010924748217 ) ) ;
#8745 = CARTESIAN_POINT ( 'NONE',  ( 1.035533905932737975, 184.1500000000000341, 4.500000000000000888 ) ) ;
#8746 = CARTESIAN_POINT ( 'NONE',  ( -5.935543223013826086, -0.8771126767608832253, 17.99999999999998934 ) ) ;
#8748 = VERTEX_POINT ( 'NONE', #9017 ) ;
#8747 = CARTESIAN_POINT ( 'NONE',  ( 2.066987299999999639, 188.4999999989075263, 6.143825827087054492 ) ) ;
#8749 = AXIS2_PLACEMENT_3D ( 'NONE', #8761, #5493, #13594 ) ;
#8750 = CARTESIAN_POINT ( 'NONE',  ( -3.420659742068472120, -4.931142898501675198, 23.50004946353776702 ) ) ;
#8751 = CARTESIAN_POINT ( 'NONE',  ( 5.558508435838260375, -2.857531096718794128, 11.63237410716304332 ) ) ;
#8752 =( NAMED_UNIT ( * ) PLANE_ANGLE_UNIT ( ) SI_UNIT ( $, .RADIAN. ) );
#8753 = CARTESIAN_POINT ( 'NONE',  ( -5.999999999999999112, 221.4150671951173592, 6.196499129422101682 ) ) ;
#8754 = CARTESIAN_POINT ( 'NONE',  ( -2.066987300000000971, 188.6499999989075036, 7.000000000000000000 ) ) ;
#8755 = CARTESIAN_POINT ( 'NONE',  ( 2.692335458626773370, 5.362264153667272382, 17.73760108194401752 ) ) ;
#8756 = CARTESIAN_POINT ( 'NONE',  ( 0.08805000471466810363, 188.9999999996602469, 9.502418226916221400 ) ) ;
#8757 = CARTESIAN_POINT ( 'NONE',  ( -4.435347140101010055, -4.403429997944535046, 5.000000000000004441 ) ) ;
#8758 = CARTESIAN_POINT ( 'NONE',  ( -7.180990026460705167, -3.384707322287646480, 17.99999999999998934 ) ) ;
#8759 = CARTESIAN_POINT ( 'NONE',  ( 1.354942164390165777E-13, -6.250000000000000888, 16.99999999999998579 ) ) ;
#8760 = CARTESIAN_POINT ( 'NONE',  ( -5.903119516422464130, -1.077859910107564545, 12.11519382448850557 ) ) ;
#8761 = CARTESIAN_POINT ( 'NONE',  ( 0.000000000000000000, 0.000000000000000000, 5.000000000000004441 ) ) ;
#8762 = VERTEX_POINT ( 'NONE', #11534 ) ;
#8763 = CARTESIAN_POINT ( 'NONE',  ( -2.066987300000000083, 187.1999999989075434, 6.143825827087054492 ) ) ;
#8764 = ADVANCED_FACE ( 'NONE', ( #13844, #9966, #11459, #2720 ), #562, .F. ) ;
#8765 = ORIENTED_EDGE ( 'NONE', *, *, #4384, .F. ) ;
#8766 = EDGE_CURVE ( 'NONE', #14218, #8478, #8515, .T. ) ;
#8767 = CARTESIAN_POINT ( 'NONE',  ( 0.000000000000000000, 0.000000000000000000, 0.000000000000000000 ) ) ;
#8768 = VECTOR ( 'NONE', #12067, 1000.000000000000000 ) ;
#8769 = EDGE_LOOP ( 'NONE', ( #7115, #6806, #11599, #10192 ) ) ;
#8770 = CARTESIAN_POINT ( 'NONE',  ( -3.632151824461228973, 4.777505256984487580, 25.50004932073311892 ) ) ;
#8771 = ORIENTED_EDGE ( 'NONE', *, *, #5042, .T. ) ;
#8772 = CARTESIAN_POINT ( 'NONE',  ( 1.461580736456473018, -1.461580736456472573, -1.649999998907525356 ) ) ;
#8773 = CARTESIAN_POINT ( 'NONE',  ( -6.176542424588096658, -0.9554180641287005615, 11.63237410716304687 ) ) ;
#8774 = CARTESIAN_POINT ( 'NONE',  ( -0.9143442643220817123, 228.2093053035189030, 10.03355751118253636 ) ) ;
#8775 = CARTESIAN_POINT ( 'NONE',  ( -0.6151877315909173305, 6.220340188096023404, 25.29906673469658784 ) ) ;
#8776 = CARTESIAN_POINT ( 'NONE',  ( -2.500000000000000000, 0.000000000000000000, 1.700000000000000178 ) ) ;
#8777 = AXIS2_PLACEMENT_3D ( 'NONE', #13536, #6397, #11153 ) ;
#8778 = CARTESIAN_POINT ( 'NONE',  ( -3.634089073485536669, 4.776071126502611008, 17.00007997643736957 ) ) ;
#8779 = ITEM_DEFINED_TRANSFORMATION ( 'NONE', 'NONE', #8843,  #14201 ) ;
#8780 = CARTESIAN_POINT ( 'NONE',  ( -6.176542424588071789, -0.9554180641288338993, 24.63237410716305575 ) ) ;
#8781 = CARTESIAN_POINT ( 'NONE',  ( -2.066987299999999639, 0.8561741729129452860, -0.9999999989075254447 ) ) ;
#8782 = CARTESIAN_POINT ( 'NONE',  ( -5.770167736194723673, 2.404664418229099265, 30.12632671364008274 ) ) ;
#8783 = CARTESIAN_POINT ( 'NONE',  ( -1.827163138824825950, 228.0559401102076151, 9.582586618047248095 ) ) ;
#8784 = VERTEX_POINT ( 'NONE', #15442 ) ;
#8785 = ORIENTED_EDGE ( 'NONE', *, *, #1894, .F. ) ;
#8786 = ADVANCED_FACE ( 'NONE', ( #8044 ), #5205, .T. ) ;
#8787 = VERTEX_POINT ( 'NONE', #6780 ) ;
#8788 = CARTESIAN_POINT ( 'NONE',  ( 5.531757352715602316, -2.326874507723326158, 30.12619317285288645 ) ) ;
#8789 = CARTESIAN_POINT ( 'NONE',  ( 0.2558939153494951824, 188.9999999999999716, 4.506307806592411147 ) ) ;
#8790 = AXIS2_PLACEMENT_3D ( 'NONE', #9322, #6790, #4469 ) ;
#8791 = ORIENTED_EDGE ( 'NONE', *, *, #939, .F. ) ;
#8792 =( GEOMETRIC_REPRESENTATION_CONTEXT ( 3 ) GLOBAL_UNCERTAINTY_ASSIGNED_CONTEXT ( ( #904 ) ) GLOBAL_UNIT_ASSIGNED_CONTEXT ( ( #8679, #12317, #12082 ) ) REPRESENTATION_CONTEXT ( 'NONE', 'WORKASPACE' ) );
#8793 = DIRECTION ( 'NONE',  ( -1.000000000000000000, 3.326610055774637112E-18, 1.062480551894331163E-17 ) ) ;
#8794 = CARTESIAN_POINT ( 'NONE',  ( 2.031800924177950305E-13, 6.000000000000000888, 23.49999999999999289 ) ) ;
#8795 = CARTESIAN_POINT ( 'NONE',  ( 3.459597053047760440, -5.206576120509801342, 23.52591457665828756 ) ) ;
#8796 = CARTESIAN_POINT ( 'NONE',  ( 0.09128442574521389297, -0.3999999999999975797, -2.551849451998178253 ) ) ;
#8797 = FACE_OUTER_BOUND ( 'NONE', #15211, .T. ) ;
#8798 = CARTESIAN_POINT ( 'NONE',  ( -6.020865209844624921, 1.681180471732039550, 5.974000980233303615 ) ) ;
#8799 = CARTESIAN_POINT ( 'NONE',  ( 0.8737888311112075312, -5.936248257219478575, 25.00344185141216613 ) ) ;
#8800 = DIRECTION ( 'NONE',  ( 0.000000000000000000, -1.000000000000000000, 0.000000000000000000 ) ) ;
#8801 = CARTESIAN_POINT ( 'NONE',  ( -1.767766952966369542, 186.0699999975965397, 8.767766952966368876 ) ) ;
#8802 = CARTESIAN_POINT ( 'NONE',  ( 0.5174937098143853609, 227.6312805367891201, 5.174508016632918483 ) ) ;
#8803 = CARTESIAN_POINT ( 'NONE',  ( -2.842171547016528965, 226.9791356524935395, 6.413666598675894726 ) ) ;
#8804 = CARTESIAN_POINT ( 'NONE',  ( -2.233311234937184420, 189.1493003526281882, 9.186062866647521474 ) ) ;
#8805 = ORIENTED_EDGE ( 'NONE', *, *, #14842, .T. ) ;
#8806 = CARTESIAN_POINT ( 'NONE',  ( -6.142908455506932874, 1.155755562476104892, 17.38482219624156855 ) ) ;
#8807 = CARTESIAN_POINT ( 'NONE',  ( 4.416779112813673080, -4.422345839825776892, 11.23774718278287743 ) ) ;
#8808 = CARTESIAN_POINT ( 'NONE',  ( -2.668367453516892418, 5.373994336898001656, 24.49999999999999289 ) ) ;
#8809 = CARTESIAN_POINT ( 'NONE',  ( 0.5042987395409762597, 5.979983180450060054, 25.37329304179976219 ) ) ;
#8810 = B_SPLINE_CURVE_WITH_KNOTS ( 'NONE', 3,
 ( #6813, #11724, #5538, #4337, #1938, #10615, #593, #12687, #12835, #9194, #3213, #3293, #1784, #5694, #12916, #11648, #9424, #15475 ),
 .UNSPECIFIED., .F., .F.,
 ( 4, 2, 2, 2, 2, 2, 2, 2, 4 ),
 ( 0.000000000000000000, 0.0003914904498596247923, 0.0007829808997192495845, 0.001174471349578874377, 0.001565961799438499169, 0.001957452249298123961, 0.002348942699157748754, 0.002740433149017373546, 0.003131923598876998338 ),
 .UNSPECIFIED. ) ;
#8811 = CARTESIAN_POINT ( 'NONE',  ( 2.421481774831334199, 227.8602969206058617, 9.007210671174304295 ) ) ;
#8812 = CARTESIAN_POINT ( 'NONE',  ( 3.254737477227991782, 5.337033878705210732, 5.873673286359927026 ) ) ;
#8813 = CARTESIAN_POINT ( 'NONE',  ( 1.767766952966368654, 1.767766952966369098, 2.200000000000000178 ) ) ;
#8814 = CYLINDRICAL_SURFACE ( 'NONE', #13776, 1.499999999999999556 ) ;
#8815 = CARTESIAN_POINT ( 'NONE',  ( 5.621197618055676415, 2.101623592078516012, 5.973980201222398811 ) ) ;
#8816 = CARTESIAN_POINT ( 'NONE',  ( -1.767766952966369765, 186.0999999999999943, 8.767766952966368876 ) ) ;
#8817 = FACE_BOUND ( 'NONE', #6553, .T. ) ;
#8818 = CARTESIAN_POINT ( 'NONE',  ( -1.690976820968455474, 227.9165037442230926, 5.998248907768082283 ) ) ;
#8819 = CARTESIAN_POINT ( 'NONE',  ( 3.796994071234844259E-16, -2.066987299999999639, -1.549999998907525045 ) ) ;
#8820 = CARTESIAN_POINT ( 'NONE',  ( 6.020822430078855980, -1.681351817312188635, 25.47408542334170889 ) ) ;
#8821 = B_SPLINE_CURVE_WITH_KNOTS ( 'NONE', 3,
 ( #6190, #15651, #11028, #126, #4753, #13875, #6348, #15010, #13563, #14848, #7448, #10231, #6428, #13726, #8809, #12292, #1630, #3858 ),
 .UNSPECIFIED., .F., .F.,
 ( 4, 2, 2, 2, 2, 2, 2, 2, 4 ),
 ( 0.003131923598876995302, 0.003523316383094312644, 0.003914709167311630419, 0.004306101951528947328, 0.004697494735746265103, 0.005088887519963582878, 0.005480280304180899786, 0.005871673088398216694, 0.006263065872615534470 ),
 .UNSPECIFIED. ) ;
#8822 = VECTOR ( 'NONE', #14728, 1000.000000000000000 ) ;
#8823 = CARTESIAN_POINT ( 'NONE',  ( -0.8561741729129455081, 2.066987299999999639, 0.3000000010924747662 ) ) ;
#8824 = CARTESIAN_POINT ( 'NONE',  ( 2.500000000000000444, 184.0500000000000114, 5.964466094067262247 ) ) ;
#8825 = CARTESIAN_POINT ( 'NONE',  ( 5.558508435838291462, -2.857531096718732400, 17.99999999999998934 ) ) ;
#8827 = EDGE_LOOP ( 'NONE', ( #11622, #15295 ) ) ;
#8826 = CARTESIAN_POINT ( 'NONE',  ( -0.8561741729129456191, 188.6999999989075150, 4.933012699999999029 ) ) ;
#8828 = CARTESIAN_POINT ( 'NONE',  ( -2.692215568229842315, -5.362327947133593398, 17.73770962164069331 ) ) ;
#8829 = ADVANCED_FACE ( 'NONE', ( #5586 ), #8531, .F. ) ;
#8830 = EDGE_CURVE ( 'NONE', #512, #13950, #77, .T. ) ;
#8831 = VECTOR ( 'NONE', #5796, 1000.000000000000000 ) ;
#8832 = CARTESIAN_POINT ( 'NONE',  ( -5.999999999999999112, 189.3270225533669020, 3.938484906660875584 ) ) ;
#8833 = CARTESIAN_POINT ( 'NONE',  ( 7.490007020835706797, -2.433650805992179755, 11.49999999999998224 ) ) ;
#8834 = CARTESIAN_POINT ( 'NONE',  ( 4.267558728637101950, 4.217879122113895818, 17.73617396794403689 ) ) ;
#8835 = CARTESIAN_POINT ( 'NONE',  ( 2.995127566766980554, 189.8664680706473007, 7.560295519963911914 ) ) ;
#8836 = CARTESIAN_POINT ( 'NONE',  ( -1.035533905932737975, 188.1499999978150584, 4.500000000000001776 ) ) ;
#8837 = CARTESIAN_POINT ( 'NONE',  ( 2.696147639476683455, 189.8139822597015609, 8.673643915089936485 ) ) ;
#8838 = CARTESIAN_POINT ( 'NONE',  ( -2.500000000000000000, 0.000000000000000000, -2.199999997815050623 ) ) ;
#8839 = DIRECTION ( 'NONE',  ( -0.9510565162951545304, 0.3090169943749447867, 0.000000000000000000 ) ) ;
#8840 = CARTESIAN_POINT ( 'NONE',  ( -0.1647438929007866704, 188.9999999999999716, 4.500000000000000000 ) ) ;
#8841 = VERTEX_POINT ( 'NONE', #1031 ) ;
#8842 = CARTESIAN_POINT ( 'NONE',  ( 0.8561741729129452860, 188.5999999989074922, 4.933012699999999029 ) ) ;
#8843 = AXIS2_PLACEMENT_3D ( 'NONE', #11250, #13863, #8800 ) ;
#8844 = VERTEX_POINT ( 'NONE', #15681 ) ;
#8845 = CARTESIAN_POINT ( 'NONE',  ( -5.409007216690583597, -2.598315788643936308, 23.88557478428062097 ) ) ;
#8846 = VECTOR ( 'NONE', #14406, 1000.000000000000000 ) ;
#8847 = ORIENTED_EDGE ( 'NONE', *, *, #8550, .T. ) ;
#8848 = CARTESIAN_POINT ( 'NONE',  ( -3.311384659207313064, 5.004923837169304335, 25.47358595436692852 ) ) ;
#8849 =( NAMED_UNIT ( * ) PLANE_ANGLE_UNIT ( ) SI_UNIT ( $, .RADIAN. ) );
#8850 = ORIENTED_EDGE ( 'NONE', *, *, #15341, .T. ) ;
#8851 = CARTESIAN_POINT ( 'NONE',  ( -0.8561741729129455081, 2.066987299999999639, -2.099999998907525089 ) ) ;
#8852 = DIRECTION ( 'NONE',  ( 1.000000000000000000, 0.000000000000000000, 0.000000000000000000 ) ) ;
#8853 = VECTOR ( 'NONE', #5861, 1000.000000000000000 ) ;
#8854 = CARTESIAN_POINT ( 'NONE',  ( 6.250000000000000888, 7.654042494670958593E-16, 0.000000000000000000 ) ) ;
#8855 = DIRECTION ( 'NONE',  ( -0.5877852522924685852, -0.8090169943749508930, 0.000000000000000000 ) ) ;
#8856 = CARTESIAN_POINT ( 'NONE',  ( -1.530808498934191571E-16, 2.500000000000000000, -0.9000000000000002442 ) ) ;
#8857 = VECTOR ( 'NONE', #9550, 1000.000000000000000 ) ;
#8858 = DIRECTION ( 'NONE',  ( 0.9510565162951500895, 0.3090169943749582204, 0.000000000000000000 ) ) ;
#8859 = CARTESIAN_POINT ( 'NONE',  ( -1.767766952966369320, 187.4300000002185129, 5.232233047033630235 ) ) ;
#8860 = CARTESIAN_POINT ( 'NONE',  ( -6.105925084677645387, -1.337450587213346642, 25.29933148907576523 ) ) ;
#8861 = CARTESIAN_POINT ( 'NONE',  ( -2.066987299999999639, 0.000000000000000000, -0.1499999989075253282 ) ) ;
#8862 = CARTESIAN_POINT ( 'NONE',  ( 5.903472034603518992, -2.056448723545135859, 10.49991780678442410 ) ) ;
#8863 = CARTESIAN_POINT ( 'NONE',  ( 3.736691294293371435, 4.695920479336417763, 12.47358595436692319 ) ) ;
#8864 = ORIENTED_EDGE ( 'NONE', *, *, #652, .T. ) ;
#8865 = VERTEX_POINT ( 'NONE', #10742 ) ;
#8866 = CIRCLE ( 'NONE', #12663, 2.499999999999999556 ) ;
#8867 = EDGE_LOOP ( 'NONE', ( #1659, #9320, #2652, #6597 ) ) ;
#8868 = EDGE_CURVE ( 'NONE', #9099, #9480, #13290, .T. ) ;
#8869 = VECTOR ( 'NONE', #11567, 1000.000000000000227 ) ;
#8870 = EDGE_LOOP ( 'NONE', ( #11701, #13255, #15338, #3040 ) ) ;
#8871 = CARTESIAN_POINT ( 'NONE',  ( 3.253823204785141421, 5.337590213880490708, 4.126941084456995590 ) ) ;
#8872 = AXIS2_PLACEMENT_3D ( 'NONE', #10684, #8474, #9494 ) ;
#8873 = EDGE_LOOP ( 'NONE', ( #6576, #10358, #8376, #1914 ) ) ;
#8874 = CARTESIAN_POINT ( 'NONE',  ( 7.347880347650999152E-16, -6.000000000000000888, 4.000000000000004441 ) ) ;
#8875 = CARTESIAN_POINT ( 'NONE',  ( 0.9735954530126567086, -6.173909381473971614, 18.26281793585244984 ) ) ;
#8876 = CARTESIAN_POINT ( 'NONE',  ( 0.000000000000000000, 6.250000000000000888, 18.99999999999998934 ) ) ;
#8877 = CARTESIAN_POINT ( 'NONE',  ( 0.5662760513513173111, -0.3999999999999906408, -2.593905796088002091 ) ) ;
#8878 = CARTESIAN_POINT ( 'NONE',  ( -2.500000000000000444, 186.6499999978150299, 5.964466094067261359 ) ) ;
#8879 = CARTESIAN_POINT ( 'NONE',  ( 0.09128442574521389297, -0.3999999999999975797, -2.551849451998178253 ) ) ;
#8880 = EDGE_CURVE ( 'NONE', #3363, #5259, #7849, .T. ) ;
#8881 = CARTESIAN_POINT ( 'NONE',  ( -2.997753866155858038, 5.484939622623821620, 10.88439807107077861 ) ) ;
#8882 = CARTESIAN_POINT ( 'NONE',  ( 2.782156709077347134, 5.316215864844083150, 10.99687951097621230 ) ) ;
#8883 = DIRECTION ( 'NONE',  ( 6.982962677686266711E-15, 0.000000000000000000, -1.000000000000000000 ) ) ;
#8884 = AXIS2_PLACEMENT_3D ( 'NONE', #10308, #15316, #15396 ) ;
#8885 = CARTESIAN_POINT ( 'NONE',  ( 1.035533905932737975, 186.5199999975966136, 4.500000000000000888 ) ) ;
#8886 = CARTESIAN_POINT ( 'NONE',  ( -1.160340649284625325, 228.7901875120212196, 8.521497460825987247 ) ) ;
#8887 = CARTESIAN_POINT ( 'NONE',  ( -2.884911204282110120, 227.0244024278241000, 6.546979792117293862 ) ) ;
#8888 = CARTESIAN_POINT ( 'NONE',  ( -1.008179592313656059, 189.0000000000697469, 9.292056966037035792 ) ) ;
#8889 = ORIENTED_EDGE ( 'NONE', *, *, #8070, .T. ) ;
#8890 = CARTESIAN_POINT ( 'NONE',  ( -3.632151824461058887, 4.777505256984618143, 6.000049320733126024 ) ) ;
#8891 = CARTESIAN_POINT ( 'NONE',  ( 4.344313232727135876, -4.493553492990087328, 10.99563030319846924 ) ) ;
#8892 = CARTESIAN_POINT ( 'NONE',  ( 0.2622538972264840673, -6.245673238944474015, 12.47385994369198059 ) ) ;
#8893 = CARTESIAN_POINT ( 'NONE',  ( 6.172614129015234319, 0.9817721000788910413, 11.76236973443872991 ) ) ;
#8894 = CARTESIAN_POINT ( 'NONE',  ( 2.129007923468051455, 227.9697339865814740, 9.329065678806253814 ) ) ;
#8895 = CARTESIAN_POINT ( 'NONE',  ( 2.996417732210567841, 5.485687819086908057, 5.613961794080714718 ) ) ;
#8896 = CARTESIAN_POINT ( 'NONE',  ( -1.461580736456472795, 1.461580736456472795, -1.849999998907525534 ) ) ;
#8897 = LINE ( 'NONE', #5544, #2337 ) ;
#8898 =( NAMED_UNIT ( * ) PLANE_ANGLE_UNIT ( ) SI_UNIT ( $, .RADIAN. ) );
#8899 = CYLINDRICAL_SURFACE ( 'NONE', #14594, 0.9999999999999998890 ) ;
#8900 = CARTESIAN_POINT ( 'NONE',  ( 2.500000000000000444, 184.7500000000000000, 8.035533905932739529 ) ) ;
#8901 = FACE_BOUND ( 'NONE', #4212, .T. ) ;
#8902 = CARTESIAN_POINT ( 'NONE',  ( -0.4523656679209748233, 227.6256624317788635, 5.158282608927489576 ) ) ;
#8903 = CARTESIAN_POINT ( 'NONE',  ( 2.066987299999999639, 2.531329380823229670E-16, -1.349999998907525534 ) ) ;
#8904 = CARTESIAN_POINT ( 'NONE',  ( -2.817313151351170220, -5.579000502529442684, 11.36762589283694425 ) ) ;
#8905 = DIRECTION ( 'NONE',  ( -0.000000000000000000, 1.000000000000000000, -0.000000000000000000 ) ) ;
#8906 = CARTESIAN_POINT ( 'NONE',  ( 2.500000000000000444, 184.7500000000000000, 8.035533905932739529 ) ) ;
#8907 = CARTESIAN_POINT ( 'NONE',  ( -5.903119516422453472, -1.077859910107617836, 18.61519382448850024 ) ) ;
#8908 = B_SPLINE_CURVE_WITH_KNOTS ( 'NONE', 3,
 ( #4320, #9488, #5753, #14171, #648, #885, #9256, #3352, #5600, #2078, #6876, #11709, #3276, #10368, #10446, #2153, #8218, #810 ),
 .UNSPECIFIED., .F., .F.,
 ( 4, 2, 2, 2, 2, 2, 2, 2, 4 ),
 ( 0.000000000000000000, 0.0003914357524127488950, 0.0007828715048254977901, 0.001174307257238246848, 0.001565743009650995580, 0.001957178762063744529, 0.002348614514476491961, 0.002740050266889240260, 0.003131486019301987691 ),
 .UNSPECIFIED. ) ;
#8910 = VERTEX_POINT ( 'NONE', #14726 ) ;
#8909 = CARTESIAN_POINT ( 'NONE',  ( 0.8561741729129457301, 189.0999999989075206, 9.066987299999999195 ) ) ;
#8911 = CARTESIAN_POINT ( 'NONE',  ( -3.882673863916308754, -4.899192824800922885, 17.02591457665827690 ) ) ;
#8912 = AXIS2_PLACEMENT_3D ( 'NONE', #13161, #6973, #10702 ) ;
#8913 = DIRECTION ( 'NONE',  ( -0.5877852522924685852, -0.8090169943749507819, 0.000000000000000000 ) ) ;
#8914 = CARTESIAN_POINT ( 'NONE',  ( -5.935543223013862502, 0.8771126767606658436, 4.867606119983655333 ) ) ;
#8915 = CARTESIAN_POINT ( 'NONE',  ( 2.494052150861849171, 189.1790225982191487, 8.847987137205636898 ) ) ;
#8916 = CARTESIAN_POINT ( 'NONE',  ( 6.176542424588125968, 0.9554180641284963915, 17.99999999999998934 ) ) ;
#8917 = CARTESIAN_POINT ( 'NONE',  ( 4.267558728637259158, -4.217879122113739498, 5.263826032055956894 ) ) ;
#8918 = CARTESIAN_POINT ( 'NONE',  ( -3.107583187530443602, 5.133966411712675537, 30.12619317285289000 ) ) ;
#8919 = DIRECTION ( 'NONE',  ( -1.000000000000000000, 0.000000000000000000, 0.000000000000000000 ) ) ;
#8920 = CARTESIAN_POINT ( 'NONE',  ( -5.746996058422751297, -1.729015645942007184, 10.49992038825521767 ) ) ;
#8921 = VERTEX_POINT ( 'NONE', #13360 ) ;
#8922 = CARTESIAN_POINT ( 'NONE',  ( -1.461580736456472795, 185.5499999989075093, 5.538419263543527649 ) ) ;
#8923 = EDGE_CURVE ( 'NONE', #13408, #5765, #3497, .T. ) ;
#8924 = ORIENTED_EDGE ( 'NONE', *, *, #9799, .T. ) ;
#8925 = CARTESIAN_POINT ( 'NONE',  ( 0.09128442572436945568, 0.4000000000000010214, 2.551849451885215725 ) ) ;
#8926 = EDGE_LOOP ( 'NONE', ( #9500, #2690 ) ) ;
#8927 = DIRECTION ( 'NONE',  ( 0.5877852522924802425, -0.8090169943749422332, 0.000000000000000000 ) ) ;
#8928 = DIRECTION ( 'NONE',  ( -0.000000000000000000, 1.000000000000000000, -0.000000000000000000 ) ) ;
#8929 = EDGE_LOOP ( 'NONE', ( #2050, #15140, #9478, #15472 ) ) ;
#8930 = CARTESIAN_POINT ( 'NONE',  ( 3.796994071234844259E-16, -2.066987299999999639, -1.749999998907525223 ) ) ;
#8931 = CARTESIAN_POINT ( 'NONE',  ( 0.7995298244854619485, 5.947211616899248376, 5.614560146198583901 ) ) ;
#8932 = CARTESIAN_POINT ( 'NONE',  ( -1.318079107690499852, 228.1589215201366869, 9.885401715239364506 ) ) ;
#8933 = CARTESIAN_POINT ( 'NONE',  ( 0.8561741729129451750, 189.3999999989075604, 4.933012699999999029 ) ) ;
#8934 = CARTESIAN_POINT ( 'NONE',  ( -2.500000000000000000, 0.000000000000000000, -0.7000000000000000666 ) ) ;
#8935 = LINE ( 'NONE', #8647, #1725 ) ;
#8936 = EDGE_CURVE ( 'NONE', #15690, #6555, #7734, .T. ) ;
#8937 = CARTESIAN_POINT ( 'NONE',  ( -4.286401442266582151, -4.198423832313145532, 11.36935038651143515 ) ) ;
#8938 = CARTESIAN_POINT ( 'NONE',  ( 2.500000000000000444, 1.035533905932737975, -0.9499999978150504010 ) ) ;
#8939 = CARTESIAN_POINT ( 'NONE',  ( 2.066987299999999639, 0.8561741729129456191, 0.3000000010924747662 ) ) ;
#8940 = CARTESIAN_POINT ( 'NONE',  ( 6.081836621194455006, -1.445163676684758425, 10.62694108445696806 ) ) ;
#8941 = FACE_OUTER_BOUND ( 'NONE', #7659, .T. ) ;
#8942 = EDGE_CURVE ( 'NONE', #5900, #8784, #12009, .T. ) ;
#8943 = ORIENTED_EDGE ( 'NONE', *, *, #11721, .T. ) ;
#8944 = EDGE_LOOP ( 'NONE', ( #11815, #13027, #394, #11006 ) ) ;
#8945 = B_SPLINE_CURVE_WITH_KNOTS ( 'NONE', 3,
 ( #12493, #4220, #6700, #5502, #7721, #11455, #10117, #5426, #6545, #1592, #6470, #5270, #11303, #11378, #558, #10271, #9089, #15201 ),
 .UNSPECIFIED., .F., .F.,
 ( 4, 2, 2, 2, 2, 2, 2, 2, 4 ),
 ( 0.000000000000000000, 0.0003914904498596247923, 0.0007829808997192493677, 0.001174471349578873943, 0.001565961799438498735, 0.001957452249298123528, 0.002348942699157747886, 0.002740433149017373112, 0.003131923598876997471 ),
 .UNSPECIFIED. ) ;
#8946 = ORIENTED_EDGE ( 'NONE', *, *, #9439, .F. ) ;
#8947 = DIRECTION ( 'NONE',  ( 0.000000000000000000, -2.775557561562887900E-16, 1.000000000000000000 ) ) ;
#8948 = CARTESIAN_POINT ( 'NONE',  ( 2.046085422626991779, 189.0000000000000568, 8.444739450853276708 ) ) ;
#8949 = ORIENTED_EDGE ( 'NONE', *, *, #10190, .T. ) ;
#8950 = CARTESIAN_POINT ( 'NONE',  ( -0.2638277032948904699, -5.995407492418041606, 5.973320552815183149 ) ) ;
#8951 = B_SPLINE_CURVE_WITH_KNOTS ( 'NONE', 1,
 ( #7239, #2454 ),
 .UNSPECIFIED., .F., .F.,
 ( 2, 2 ),
 ( 0.000000000000000000, 1.000000000000000000 ),
 .UNSPECIFIED. ) ;
#8952 = CARTESIAN_POINT ( 'NONE',  ( 0.8736516769107001146, -5.936271176698233454, 30.49606771578675435 ) ) ;
#8953 = CARTESIAN_POINT ( 'NONE',  ( -4.435347140101089991, 4.403429997944455110, 31.13063932754212004 ) ) ;
#8954 = CARTESIAN_POINT ( 'NONE',  ( -2.500000000000000000, -1.035533905932739307, -2.250000000000000888 ) ) ;
#8955 = CARTESIAN_POINT ( 'NONE',  ( -1.035533905932737975, 187.3499999978151038, 4.500000000000000888 ) ) ;
#8956 = CARTESIAN_POINT ( 'NONE',  ( 2.500000000000000444, -1.035533905932737309, 1.256999999978150706 ) ) ;
#8957 = EDGE_CURVE ( 'NONE', #4790, #12014, #8610, .T. ) ;
#8958 = FACE_OUTER_BOUND ( 'NONE', #7195, .T. ) ;
#8959 = AXIS2_PLACEMENT_3D ( 'NONE', #3861, #11107, #13565 ) ;
#8960 = CARTESIAN_POINT ( 'NONE',  ( -2.500000000000000444, 186.7699999975965568, 7.000000000000000000 ) ) ;
#8961 = CARTESIAN_POINT ( 'NONE',  ( 1.747590535343585438, 228.0744605602133674, 9.637048244069795544 ) ) ;
#8962 = CARTESIAN_POINT ( 'NONE',  ( -2.381136272098726803, 226.7019369474745361, 5.597090573316407358 ) ) ;
#8963 = VERTEX_POINT ( 'NONE', #9795 ) ;
#8964 = CARTESIAN_POINT ( 'NONE',  ( 0.4428048500434558221, -2.464588252924116318, -2.500827920915885461 ) ) ;
#8965 = EDGE_CURVE ( 'NONE', #1678, #7319, #5655, .T. ) ;
#8966 = ORIENTED_EDGE ( 'NONE', *, *, #12512, .F. ) ;
#8967 = CARTESIAN_POINT ( 'NONE',  ( -5.770167736194681041, 2.404664418229203626, 17.12632671364005787 ) ) ;
#8968 = CARTESIAN_POINT ( 'NONE',  ( 4.290381260516300088, -4.545736887716183894, 10.88482219624156144 ) ) ;
#8969 = DIRECTION ( 'NONE',  ( -0.000000000000000000, -1.000000000000000000, -0.000000000000000000 ) ) ;
#8970 = DIRECTION ( 'NONE',  ( 0.000000000000000000, 0.000000000000000000, 1.000000000000000000 ) ) ;
#8971 = VECTOR ( 'NONE', #13687, 1000.000000000000000 ) ;
#8972 = CARTESIAN_POINT ( 'NONE',  ( 1.295909982280349482, 228.1605777260576531, 9.890276522793730152 ) ) ;
#8973 = EDGE_CURVE ( 'NONE', #14218, #5590, #9694, .T. ) ;
#8974 = CARTESIAN_POINT ( 'NONE',  ( 3.107278289587092512, -5.134157760522109371, 23.62635295315576656 ) ) ;
#8975 = CARTESIAN_POINT ( 'NONE',  ( -2.066987299999999639, 0.000000000000000000, -2.549999998907525711 ) ) ;
#8976 = CARTESIAN_POINT ( 'NONE',  ( -2.500000000000000888, 188.3999999999999773, 7.000000000000000000 ) ) ;
#8977 = CARTESIAN_POINT ( 'NONE',  ( 5.915755444410787156, 1.003187219519937168, 5.503120489023787698 ) ) ;
#8978 = SHAPE_REPRESENTATION ( 'finger base', ( #14201 ), #4042 ) ;
#8979 = CARTESIAN_POINT ( 'NONE',  ( 1.767766952966368654, 185.5000000000000000, 8.767766952966368876 ) ) ;
#8980 = CARTESIAN_POINT ( 'NONE',  ( -0.7022813136239680620, 227.6507649362739585, 5.230780073663146013 ) ) ;
#8981 = CARTESIAN_POINT ( 'NONE',  ( -1.265664690411614835E-16, 2.066987299999999639, -2.749999998907525001 ) ) ;
#8982 = CIRCLE ( 'NONE', #7953, 1.500000000000001776 ) ;
#8983 = B_SPLINE_CURVE_WITH_KNOTS ( 'NONE', 3,
 ( #10314, #1559, #13734, #1790, #4185, #10080, #12614, #6666, #6586, #5316, #12377, #12693, #7611, #12458, #11268, #368, #10161, #15167 ),
 .UNSPECIFIED., .F., .F.,
 ( 4, 2, 2, 2, 2, 2, 2, 2, 4 ),
 ( 0.000000000000000000, 0.0003914357524127487866, 0.0007828715048254975733, 0.001174307257238246414, 0.001565743009650995147, 0.001957178762063744096, 0.002348614514476492828, 0.002740050266889241561, 0.003131486019301990293 ),
 .UNSPECIFIED. ) ;
#8984 = CARTESIAN_POINT ( 'NONE',  ( -3.458467055437238091, -5.207305717053865912, 10.52640428276697371 ) ) ;
#8985 = CARTESIAN_POINT ( 'NONE',  ( 3.796994071234844259E-16, -2.066987299999999639, 1.450000001092474733 ) ) ;
#8986 = CARTESIAN_POINT ( 'NONE',  ( 2.500000000000000444, 184.0000000000000000, 7.000000000000000000 ) ) ;
#8987 = CARTESIAN_POINT ( 'NONE',  ( -4.286401442266688733, 4.198423832313033621, 17.99999999999998934 ) ) ;
#8988 = EDGE_CURVE ( 'NONE', #15705, #3990, #9078, .T. ) ;
#8990 = EDGE_LOOP ( 'NONE', ( #7056, #10131, #11508, #11118 ) ) ;
#8989 = CARTESIAN_POINT ( 'NONE',  ( 0.8561741729129452860, 189.3999999989075889, 4.933012699999999029 ) ) ;
#8991 =( BOUNDED_SURFACE ( )  B_SPLINE_SURFACE ( 1, 2, ( 
 ( #5444, #15217, #2969, #15455, #7818, #4400, #14017, #6641, #9326, #7976, #2076, #12973, #9254, #6949, #6717, #12740, #13857, #12669, #10522, #14168, #11781, #3123, #14088, #5518, #808, #10366, #1842, #575, #646, #7899, #11549, #4317, #5598, #730, #1766, #9178, #12816, #15376, #1998, #4238, #11628, #10444, #1921, #11471, #3273, #6794, #4472, #883, #15298, #3199, #9106, #8057, #10289, #5751, #6873, #11707, #5674, #15142, #8135, #13935, #10595, #14317, #11939, #7101, #7025, #1045, #3588, #88, #12180, #8380, #15691, #10753, #14240, #8462, #5830, #10991, #3424, #5908, #15612, #11853, #4713, #13296, #3667, #8295, #12098, #3350, #8216, #2232, #1278, #8541, #13369, #2312, #5987, #13218, #4795, #13132, #10830, #9564, #1197, #14404, #9486 ),
 ( #9650, #4631, #13052, #2393, #6152, #3511, #2478, #9732, #9404, #964, #7338, #7261, #2150, #14491, #10675, #6071, #10915, #7184, #13, #12022, #1122, #15535, #4875, #14570, #12570, #2558, #14656, #14812, #11146, #5185, #5269, #3743, #6389, #325, #1356, #11066, #1668, #13529, #9961, #13763, #6469, #6308, #3975, #2872, #248, #9883, #167, #8620, #3823, #14736, #7489, #12334, #11223, #11377, #7415, #5028, #10116, #12415, #6231, #4956, #10039, #1513, #13455, #6544, #7720, #9806, #7644, #2635, #5108, #1431, #8696, #3897, #4060, #2715, #8772, #13684, #8930, #11302, #12257, #13603, #14969, #7567, #14888, #8851, #12491, #1591, #2794, #399, #5425, #480, #6622, #1747, #1825, #707, #15576, #13915, #11454, #6698, #11900, #4219, #9234 ) ),
 .UNSPECIFIED., .F., .F., .F. ) 
 B_SPLINE_SURFACE_WITH_KNOTS ( ( 2, 2 ),
 ( 3, 2, 2, 2, 2, 2, 2, 2, 2, 2, 2, 2, 2, 2, 2, 2, 2, 2, 2, 2, 2, 2, 2, 2, 2, 2, 2, 2, 2, 2, 2, 2, 2, 2, 2, 2, 2, 2, 2, 2, 2, 2, 2, 2, 2, 2, 2, 2, 2, 2, 3 ),
 ( 0.000000000000000000, 1.000000000000000000 ),
 ( 0.000000000000000000, 0.01785714285714285615, 0.03571428571428571230, 0.05357142857142856845, 0.07142857142857142461, 0.08928571428571428770, 0.1071428571428571369, 0.1250000000000000000, 0.1428571428571428492, 0.1607142857142857262, 0.1785714285714285754, 0.1964285714285714246, 0.2142857142857142738, 0.2321428571428571508, 0.2500000000000000000, 0.2678571428571428492, 0.2857142857142856984, 0.3035714285714285476, 0.3214285714285714524, 0.3392857142857143016, 0.3571428571428571508, 0.3750000000000000000, 0.3928571428571428492, 0.4107142857142856984, 0.4285714285714285476, 0.4464285714285714524, 0.4642857142857143016, 0.4821428571428571508, 0.5000000000000000000, 0.5178571428571429047, 0.5357142857142856984, 0.5535714285714286031, 0.5714285714285713969, 0.5892857142857143016, 0.6071428571428570953, 0.6250000000000000000, 0.6428571428571429047, 0.6607142857142856984, 0.6785714285714286031, 0.6964285714285713969, 0.7142857142857143016, 0.7321428571428570953, 0.7500000000000000000, 0.7678571428571429047, 0.7857142857142856984, 0.8035714285714286031, 0.8214285714285713969, 0.8392857142857143016, 0.8571428571428570953, 0.8750000000000000000, 0.8928571428571429047 ),
 .UNSPECIFIED. ) 
 GEOMETRIC_REPRESENTATION_ITEM ( )  RATIONAL_B_SPLINE_SURFACE ( (
 ( 1.000000000000000000, 0.9238795325112867385, 1.000000000000000000, 0.9238795325112867385, 1.000000000000000000, 0.9238795325112867385, 1.000000000000000000, 0.9238795325112867385, 1.000000000000000000, 0.9238795325112867385, 1.000000000000000000, 0.9238795325112867385, 1.000000000000000000, 0.9238795325112867385, 1.000000000000000000, 0.9238795325112867385, 1.000000000000000000, 0.9238795325112867385, 1.000000000000000000, 0.9238795325112867385, 1.000000000000000000, 0.9238795325112867385, 1.000000000000000000, 0.9238795325112867385, 1.000000000000000000, 0.9238795325112867385, 1.000000000000000000, 0.9238795325112867385, 1.000000000000000000, 0.9238795325112867385, 1.000000000000000000, 0.9238795325112867385, 1.000000000000000000, 0.9238795325112867385, 1.000000000000000000, 0.9238795325112867385, 1.000000000000000000, 0.9238795325112867385, 1.000000000000000000, 0.9238795325112867385, 1.000000000000000000, 0.9238795325112867385, 1.000000000000000000, 0.9238795325112867385, 1.000000000000000000, 0.9238795325112867385, 1.000000000000000000, 0.9238795325112867385, 1.000000000000000000, 0.9238795325112867385, 1.000000000000000000, 0.9238795325112867385, 1.000000000000000000, 0.9238795325112867385, 1.000000000000000000, 0.9238795325112867385, 1.000000000000000000, 0.9238795325112867385, 1.000000000000000000, 0.9238795325112867385, 1.000000000000000000, 0.9238795325112867385, 1.000000000000000000, 0.9238795325112867385, 1.000000000000000000, 0.9238795325112867385, 1.000000000000000000, 0.9238795325112867385, 1.000000000000000000, 0.9238795325112867385, 1.000000000000000000, 0.9238795325112867385, 1.000000000000000000, 0.9238795325112867385, 1.000000000000000000, 0.9238795325112867385, 1.000000000000000000, 0.9238795325112867385, 1.000000000000000000, 0.9238795325112867385, 1.000000000000000000, 0.9238795325112867385, 1.000000000000000000, 0.9238795325112867385, 1.000000000000000000, 0.9238795325112867385, 1.000000000000000000, 0.9238795325112867385, 1.000000000000000000, 0.9238795325112867385, 1.000000000000000000, 0.9238795325112867385, 1.000000000000000000, 0.9238795325112867385, 1.000000000000000000, 0.9238795325112867385, 1.000000000000000000, 0.9238795325112867385, 1.000000000000000000, 0.9238795325112867385, 1.000000000000000000),
 ( 1.000000000000000000, 0.9238795325112867385, 1.000000000000000000, 0.9238795325112867385, 1.000000000000000000, 0.9238795325112867385, 1.000000000000000000, 0.9238795325112867385, 1.000000000000000000, 0.9238795325112867385, 1.000000000000000000, 0.9238795325112867385, 1.000000000000000000, 0.9238795325112867385, 1.000000000000000000, 0.9238795325112867385, 1.000000000000000000, 0.9238795325112867385, 1.000000000000000000, 0.9238795325112867385, 1.000000000000000000, 0.9238795325112867385, 1.000000000000000000, 0.9238795325112867385, 1.000000000000000000, 0.9238795325112867385, 1.000000000000000000, 0.9238795325112867385, 1.000000000000000000, 0.9238795325112867385, 1.000000000000000000, 0.9238795325112867385, 1.000000000000000000, 0.9238795325112867385, 1.000000000000000000, 0.9238795325112867385, 1.000000000000000000, 0.9238795325112867385, 1.000000000000000000, 0.9238795325112867385, 1.000000000000000000, 0.9238795325112867385, 1.000000000000000000, 0.9238795325112867385, 1.000000000000000000, 0.9238795325112867385, 1.000000000000000000, 0.9238795325112867385, 1.000000000000000000, 0.9238795325112867385, 1.000000000000000000, 0.9238795325112867385, 1.000000000000000000, 0.9238795325112867385, 1.000000000000000000, 0.9238795325112867385, 1.000000000000000000, 0.9238795325112867385, 1.000000000000000000, 0.9238795325112867385, 1.000000000000000000, 0.9238795325112867385, 1.000000000000000000, 0.9238795325112867385, 1.000000000000000000, 0.9238795325112867385, 1.000000000000000000, 0.9238795325112867385, 1.000000000000000000, 0.9238795325112867385, 1.000000000000000000, 0.9238795325112867385, 1.000000000000000000, 0.9238795325112867385, 1.000000000000000000, 0.9238795325112867385, 1.000000000000000000, 0.9238795325112867385, 1.000000000000000000, 0.9238795325112867385, 1.000000000000000000, 0.9238795325112867385, 1.000000000000000000, 0.9238795325112867385, 1.000000000000000000, 0.9238795325112867385, 1.000000000000000000, 0.9238795325112867385, 1.000000000000000000, 0.9238795325112867385, 1.000000000000000000, 0.9238795325112867385, 1.000000000000000000, 0.9238795325112867385, 1.000000000000000000, 0.9238795325112867385, 1.000000000000000000, 0.9238795325112867385, 1.000000000000000000, 0.9238795325112867385, 1.000000000000000000) ) ) 
 REPRESENTATION_ITEM ( '' )  SURFACE ( )  );
#8992 = CARTESIAN_POINT ( 'NONE',  ( -2.668367453516752974, -5.373994336898072710, 17.86760611998364823 ) ) ;
#8993 = DIRECTION ( 'NONE',  ( 0.000000000000000000, 0.000000000000000000, -1.000000000000000000 ) ) ;
#8994 = CARTESIAN_POINT ( 'NONE',  ( -8.250000000000003553, 3.401296724241641415E-14, 2.000000000000001776 ) ) ;
#8995 =( NAMED_UNIT ( * ) SI_UNIT ( $, .STERADIAN. ) SOLID_ANGLE_UNIT ( ) );
#8996 = CARTESIAN_POINT ( 'NONE',  ( 3.003420313107258988, 189.8839437108406969, 7.169374865749266412 ) ) ;
#8997 = CARTESIAN_POINT ( 'NONE',  ( 5.131373506000599605, 7.062729720844090231, 5.000000000000004441 ) ) ;
#8998 = CARTESIAN_POINT ( 'NONE',  ( 1.513225566872929750, 189.7309853354881852, 9.978542870372216100 ) ) ;
#8999 = LINE ( 'NONE', #1889, #5715 ) ;
#9000 = CARTESIAN_POINT ( 'NONE',  ( -3.061616997868391523E-16, 182.0000000000000000, -7.000000000000000000 ) ) ;
#9001 = CARTESIAN_POINT ( 'NONE',  ( -5.317509234263900098, -2.779225709351108797, 11.49999999999998224 ) ) ;
#9002 = EDGE_LOOP ( 'NONE', ( #12153, #9646 ) ) ;
#9003 = CARTESIAN_POINT ( 'NONE',  ( -1.461580736456473462, 188.1499999989075320, 8.461580736456472351 ) ) ;
#9004 = AXIS2_PLACEMENT_3D ( 'NONE', #5339, #10260, #9081 ) ;
#9005 = VERTEX_POINT ( 'NONE', #13591 ) ;
#9006 = CYLINDRICAL_SURFACE ( 'NONE', #4527, 1.000000000000000666 ) ;
#9007 = ORIENTED_EDGE ( 'NONE', *, *, #11780, .T. ) ;
#9008 = DIRECTION ( 'NONE',  ( 0.9510565162951500895, 0.3090169943749582204, 0.000000000000000000 ) ) ;
#9009 = FACE_OUTER_BOUND ( 'NONE', #1892, .T. ) ;
#9010 = EDGE_LOOP ( 'NONE', ( #2554, #2569, #2570, #769 ) ) ;
#9011 = LINE ( 'NONE', #556, #1057 ) ;
#9012 = CARTESIAN_POINT ( 'NONE',  ( 0.8738118504725739255, 5.936246475285030577, 5.503572421742425114 ) ) ;
#9013 = FACE_OUTER_BOUND ( 'NONE', #8333, .T. ) ;
#9014 = CARTESIAN_POINT ( 'NONE',  ( 1.035533905932739085, -2.500000000000000000, -2.049999999999999822 ) ) ;
#9015 = EDGE_CURVE ( 'NONE', #3400, #11831, #184, .T. ) ;
#9016 = CARTESIAN_POINT ( 'NONE',  ( -6.176542424588105540, -0.9554180641286327269, 5.000000000000004441 ) ) ;
#9017 = CARTESIAN_POINT ( 'NONE',  ( 0.000000000000000000, 0.4000000000000062395, -2.450963827680254337 ) ) ;
#9018 = CONTEXT_DEPENDENT_SHAPE_REPRESENTATION ( #1307, #937 ) ;
#9019 = CARTESIAN_POINT ( 'NONE',  ( 6.176542424588136626, 0.9554180641284277797, 24.49999999999999289 ) ) ;
#9020 = CARTESIAN_POINT ( 'NONE',  ( -2.066987299999999195, -0.8561741729129466183, -0.09999999890752520049 ) ) ;
#9021 = CARTESIAN_POINT ( 'NONE',  ( -0.1306394121199157821, 6.250000000000001776, 30.00000000000000355 ) ) ;
#9022 = AXIS2_PLACEMENT_3D ( 'NONE', #6901, #11732, #6821 ) ;
#9023 = ORIENTED_EDGE ( 'NONE', *, *, #5808, .T. ) ;
#9024 = EDGE_LOOP ( 'NONE', ( #2388, #13092 ) ) ;
#9025 = ORIENTED_EDGE ( 'NONE', *, *, #11241, .T. ) ;
#9026 = CARTESIAN_POINT ( 'NONE',  ( 4.435347140100978081, -4.403429997944567020, 18.13234125634167526 ) ) ;
#9027 = CARTESIAN_POINT ( 'NONE',  ( 13.50000000000000000, 0.000000000000000000, -8.673617379884035472E-16 ) ) ;
#9028 = VERTEX_POINT ( 'NONE', #463 ) ;
#9029 = CYLINDRICAL_SURFACE ( 'NONE', #10154, 1.499999999999999556 ) ;
#9030 = CARTESIAN_POINT ( 'NONE',  ( 0.2619041840696289536, -6.245686665308496366, 17.02605849433793850 ) ) ;
#9031 = ADVANCED_FACE ( 'NONE', ( #5336 ), #3456, .T. ) ;
#9032 = CARTESIAN_POINT ( 'NONE',  ( -5.746996058422793929, 1.729015645941861079, 6.000079611744768115 ) ) ;
#9033 = CARTESIAN_POINT ( 'NONE',  ( 0.000000000000000000, 6.250000000000000888, 18.99999999999998934 ) ) ;
#9034 = CARTESIAN_POINT ( 'NONE',  ( 2.500000000000000444, 184.7499999978150527, 5.964466094067262247 ) ) ;
#9035 = CARTESIAN_POINT ( 'NONE',  ( 2.449293598294706513E-15, 0.000000000000000000, 20.00000000000000000 ) ) ;
#9036 = EDGE_CURVE ( 'NONE', #4157, #8538, #1304, .T. ) ;
#9037 = DIRECTION ( 'NONE',  ( 0.8090169943749421222, 0.5877852522924802425, 0.000000000000000000 ) ) ;
#9038 = CARTESIAN_POINT ( 'NONE',  ( -9.750000000000003553, 106.0000000000000142, -3.401296724241641415E-14 ) ) ;
#9039 = CARTESIAN_POINT ( 'NONE',  ( -1.767766952966369320, 186.6699999975965625, 5.232233047033630235 ) ) ;
#9040 = CARTESIAN_POINT ( 'NONE',  ( -1.052533753945321227, 228.8137749680355455, 8.589619379135912780 ) ) ;
#9041 = CARTESIAN_POINT ( 'NONE',  ( -2.440032737085090275, 227.8520529458832300, 8.982935890751354790 ) ) ;
#9042 = VERTEX_POINT ( 'NONE', #5510 ) ;
#9043 = CARTESIAN_POINT ( 'NONE',  ( -4.286401442266640771, 4.198423832313082471, 11.49999999999998224 ) ) ;
#9044 = VECTOR ( 'NONE', #12397, 1000.000000000000000 ) ;
#9045 = VERTEX_POINT ( 'NONE', #4072 ) ;
#9046 = CARTESIAN_POINT ( 'NONE',  ( -0.1323736289504294505, 6.250000000000000000, 12.49999999999997335 ) ) ;
#9047 = CARTESIAN_POINT ( 'NONE',  ( 7.490007020835748541, -2.433650805992050969, 24.49999999999999289 ) ) ;
#9048 = CARTESIAN_POINT ( 'NONE',  ( -2.782769401326385061, 5.315896561274740861, 23.99571079637979665 ) ) ;
#9049 = CARTESIAN_POINT ( 'NONE',  ( 5.616116467183629446, 2.743044348085603712, 12.00425949503009448 ) ) ;
#9050 = CARTESIAN_POINT ( 'NONE',  ( 1.232202550405030683, 228.1699143606124380, 9.917725425114751303 ) ) ;
#9051 = CARTESIAN_POINT ( 'NONE',  ( 2.692143549875295250, -5.362363179736532537, 24.23805675996853992 ) ) ;
#9052 = CARTESIAN_POINT ( 'NONE',  ( 3.459597053047814175, -5.206576120509766703, 17.02591457665827690 ) ) ;
#9053 = AXIS2_PLACEMENT_3D ( 'NONE', #11814, #919, #14126 ) ;
#9054 = CARTESIAN_POINT ( 'NONE',  ( -1.461580736456472351, -1.461580736456473018, -1.649999998907525356 ) ) ;
#9055 = CARTESIAN_POINT ( 'NONE',  ( -3.312341048453377734, -5.004306261885516527, 31.97398020122239259 ) ) ;
#9056 =( LENGTH_UNIT ( ) NAMED_UNIT ( * ) SI_UNIT ( .MILLI., .METRE. ) );
#9057 = CARTESIAN_POINT ( 'NONE',  ( 2.500000000000000000, 188.7999999999999829, 7.000000000000000000 ) ) ;
#9058 = CARTESIAN_POINT ( 'NONE',  ( -2.500000000000000888, 187.6500000000000341, 8.035533905932737753 ) ) ;
#9059 = CARTESIAN_POINT ( 'NONE',  ( -1.740752211025599738, 227.9442165381023528, 6.078285037125840340 ) ) ;
#9060 = CARTESIAN_POINT ( 'NONE',  ( 6.155973317223314645, -1.081218830693557287, 17.49691356133953590 ) ) ;
#9061 = CARTESIAN_POINT ( 'NONE',  ( 6.155912734541165499, -1.081577393120706887, 25.00389213124970311 ) ) ;
#9062 = CARTESIAN_POINT ( 'NONE',  ( 3.796994071234844259E-16, -2.066987299999999639, -0.1499999989075253282 ) ) ;
#9063 = ADVANCED_FACE ( 'NONE', ( #8941 ), #7890, .T. ) ;
#9064 = CARTESIAN_POINT ( 'NONE',  ( -1.035533905932739529, 185.3499999999999659, 9.500000000000003553 ) ) ;
#9065 = CARTESIAN_POINT ( 'NONE',  ( -4.743384504624081899E-17, 187.2999999978150356, 4.500000000000000000 ) ) ;
#9067 = ORIENTED_EDGE ( 'NONE', *, *, #3958, .T. ) ;
#9066 = CARTESIAN_POINT ( 'NONE',  ( 2.066987300000000083, 186.8499999989075206, 7.000000000000000000 ) ) ;
#9068 = DIRECTION ( 'NONE',  ( 0.000000000000000000, 0.000000000000000000, -1.000000000000000000 ) ) ;
#9069 = CARTESIAN_POINT ( 'NONE',  ( 5.783198643800806948, -1.602922020054565078, 17.02622176056705783 ) ) ;
#9070 =( BOUNDED_CURVE ( )  B_SPLINE_CURVE ( 2, ( #11830, #15429, #9304, #1973, #5803, #701, #4292, #1895, #6850 ),
 .UNSPECIFIED., .F., .F. ) 
 B_SPLINE_CURVE_WITH_KNOTS ( ( 3, 2, 2, 2, 3 ),
 ( 0.07142857142857142461, 0.08928571428571428770, 0.1071428571428571369, 0.1250000000000000000, 0.1428571428571428492 ),
 .UNSPECIFIED. ) 
 CURVE ( )  GEOMETRIC_REPRESENTATION_ITEM ( )  RATIONAL_B_SPLINE_CURVE ( ( 1.000000000000000000, 0.9238795325112867385, 1.000000000000000000, 0.9238795325112867385, 1.000000000000000000, 0.9238795325112867385, 1.000000000000000000, 0.9238795325112867385, 1.000000000000000000 ) ) 
 REPRESENTATION_ITEM ( '' )  );
#9071 = CARTESIAN_POINT ( 'NONE',  ( -5.999999999999999112, 185.8606548077538321, 9.048340948986950849 ) ) ;
#9072 = CARTESIAN_POINT ( 'NONE',  ( 0.000000000000000000, 0.000000000000000000, 2.500000000000000000 ) ) ;
#9073 = EDGE_CURVE ( 'NONE', #2326, #2929, #14334, .T. ) ;
#9074 = CARTESIAN_POINT ( 'NONE',  ( 2.463761206207551346, 189.9754024155355694, 5.513296855513769579 ) ) ;
#9075 = CARTESIAN_POINT ( 'NONE',  ( 0.01439699119390668372, -0.3999999999999975797, -2.504551029406990370 ) ) ;
#9076 = CARTESIAN_POINT ( 'NONE',  ( -5.931817299736851901, -0.9033986943602198005, 5.262290378359327114 ) ) ;
#9077 = AXIS2_PLACEMENT_3D ( 'NONE', #3075, #603, #12697 ) ;
#9078 = LINE ( 'NONE', #8758, #8220 ) ;
#9079 = CARTESIAN_POINT ( 'NONE',  ( 6.020822430078800025, -1.681351817312382702, 5.974085423341712442 ) ) ;
#9080 = CARTESIAN_POINT ( 'NONE',  ( -1.105332846508322361E-14, 0.4000000000000061284, 2.451551129619757408 ) ) ;
#9081 = DIRECTION ( 'NONE',  ( 0.000000000000000000, 0.000000000000000000, 1.000000000000000000 ) ) ;
#9082 = ORIENTED_EDGE ( 'NONE', *, *, #13102, .T. ) ;
#9083 = CARTESIAN_POINT ( 'NONE',  ( -0.8561741729129457301, 186.0999999989074922, 4.933012699999999029 ) ) ;
#9084 = ORIENTED_EDGE ( 'NONE', *, *, #14690, .T. ) ;
#9085 = LINE ( 'NONE', #2788, #2493 ) ;
#9086 = ORIENTED_EDGE ( 'NONE', *, *, #8274, .T. ) ;
#9087 = CARTESIAN_POINT ( 'NONE',  ( -5.935543223013831415, 0.8771126767608680153, 24.49999999999999289 ) ) ;
#9088 = CARTESIAN_POINT ( 'NONE',  ( -5.842988226680558839, -1.369004370660723779, 30.12619317285289711 ) ) ;
#9089 = CARTESIAN_POINT ( 'NONE',  ( -0.1306497350715971340, 6.000000000000004441, 16.99999999999998579 ) ) ;
#9090 = CYLINDRICAL_SURFACE ( 'NONE', #4378, 1.000000000000000222 ) ;
#9091 = CARTESIAN_POINT ( 'NONE',  ( -1.035533905932738197, -2.500000000000000000, -0.5500000000000001554 ) ) ;
#9092 = CARTESIAN_POINT ( 'NONE',  ( 0.1306497350718684169, -6.000000000000000000, 16.99999999999998934 ) ) ;
#9093 = CARTESIAN_POINT ( 'NONE',  ( -4.142620314836461759, 4.341347824677426637, 17.38557478428062097 ) ) ;
#9094 = DIRECTION ( 'NONE',  ( -0.9510565162951544194, 0.3090169943749447312, 0.000000000000000000 ) ) ;
#9095 = CARTESIAN_POINT ( 'NONE',  ( -0.8561741729129455081, 2.066987299999999639, -1.899999998907525134 ) ) ;
#9096 = CARTESIAN_POINT ( 'NONE',  ( -0.1960076320828026963, 228.2536001344089982, 10.16376666290868336 ) ) ;
#9097 = AXIS2_PLACEMENT_3D ( 'NONE', #14657, #9807, #9651 ) ;
#9098 = ORIENTED_EDGE ( 'NONE', *, *, #11370, .F. ) ;
#9099 = VERTEX_POINT ( 'NONE', #638 ) ;
#9100 = EDGE_LOOP ( 'NONE', ( #13147, #1780 ) ) ;
#9101 = CARTESIAN_POINT ( 'NONE',  ( 4.416397290909879203, -4.422724436066459930, 18.26379616840804943 ) ) ;
#9102 = LINE ( 'NONE', #12813, #15725 ) ;
#9103 = ORIENTED_EDGE ( 'NONE', *, *, #1035, .T. ) ;
#9104 = AXIS2_PLACEMENT_3D ( 'NONE', #14998, #12519, #1618 ) ;
#9105 = CARTESIAN_POINT ( 'NONE',  ( 5.915699123067186704, -1.003533581835382327, 18.50389795015985328 ) ) ;
#9106 = CARTESIAN_POINT ( 'NONE',  ( -1.767766952966369098, 1.767766952966369098, -0.6999999978150504010 ) ) ;
#9107 = VECTOR ( 'NONE', #10101, 1000.000000000000114 ) ;
#9108 = CARTESIAN_POINT ( 'NONE',  ( -5.931734679891459194, 0.9039278060243389756, 5.263826032055957782 ) ) ;
#9109 = DIRECTION ( 'NONE',  ( 0.000000000000000000, 0.000000000000000000, -1.000000000000000000 ) ) ;
#9110 = CARTESIAN_POINT ( 'NONE',  ( 1.035533905932737753, 189.6499999978150868, 4.500000000000000888 ) ) ;
#9111 = CARTESIAN_POINT ( 'NONE',  ( 5.931828553037982843, -0.9033193133618682147, 11.76194324003145653 ) ) ;
#9112 = CARTESIAN_POINT ( 'NONE',  ( 5.783198643800785632, 1.602922020054637908, 18.97377823943291730 ) ) ;
#9113 = DIRECTION ( 'NONE',  ( 1.000000000000000000, 0.000000000000000000, 1.047444401652940007E-14 ) ) ;
#9114 = CARTESIAN_POINT ( 'NONE',  ( 2.500000000000000000, 188.7699999975965568, 7.000000000000000000 ) ) ;
#9115 = CARTESIAN_POINT ( 'NONE',  ( -1.886200273035058439, 228.4697824026276294, 7.596149230188033563 ) ) ;
#9116 = CARTESIAN_POINT ( 'NONE',  ( -2.898051746902431614, 227.0396595591786308, 6.591911377507474690 ) ) ;
#9117 = AXIS2_PLACEMENT_3D ( 'NONE', #4608, #7076, #13651 ) ;
#9118 = ORIENTED_EDGE ( 'NONE', *, *, #3461, .F. ) ;
#9119 = EDGE_CURVE ( 'NONE', #11432, #4730, #4557, .T. ) ;
#9120 = CARTESIAN_POINT ( 'NONE',  ( 0.1601274832639230095, -2.498925885410993697, -2.500580210930910319 ) ) ;
#9121 = ORIENTED_EDGE ( 'NONE', *, *, #5139, .F. ) ;
#9122 = EDGE_CURVE ( 'NONE', #6446, #14180, #12026, .T. ) ;
#9123 = CARTESIAN_POINT ( 'NONE',  ( -5.131373506000878493, 7.062729720843910819, 24.49999999999999289 ) ) ;
#9124 = CARTESIAN_POINT ( 'NONE',  ( 1.354942165116848791E-13, 6.250000000000000888, 16.99999999999998579 ) ) ;
#9125 = CARTESIAN_POINT ( 'NONE',  ( 6.000000000000000000, 7.347880794884118750E-16, 0.000000000000000000 ) ) ;
#9126 = CARTESIAN_POINT ( 'NONE',  ( 5.616089948629776174, 2.743103014345448454, 23.99563030319847101 ) ) ;
#9127 = FACE_OUTER_BOUND ( 'NONE', #4130, .T. ) ;
#9128 = CARTESIAN_POINT ( 'NONE',  ( 2.817313151351108047, 5.579000502529472882, 5.000000000000004441 ) ) ;
#9129 = CARTESIAN_POINT ( 'NONE',  ( -4.154121946520942465, -4.670585111242909981, 18.79887838423337953 ) ) ;
#9130 = CARTESIAN_POINT ( 'NONE',  ( 2.500000000000000444, 1.035533905932737975, -1.050000000000000044 ) ) ;
#9131 = CARTESIAN_POINT ( 'NONE',  ( 4.005785023174460058, 4.467917056767396033, 4.200479458972858460 ) ) ;
#9132 = CARTESIAN_POINT ( 'NONE',  ( -2.500000000000000888, 188.3999999999999773, 7.000000000000000000 ) ) ;
#9133 = CARTESIAN_POINT ( 'NONE',  ( -0.6404026449181154934, 227.6435107573390724, 5.209829591148105621 ) ) ;
#9134 = FACE_BOUND ( 'NONE', #7370, .T. ) ;
#9135 = CARTESIAN_POINT ( 'NONE',  ( -5.935543223013842962, 0.8771126767608004027, 18.13236078583909361 ) ) ;
#9136 = EDGE_CURVE ( 'NONE', #7504, #12468, #1990, .T. ) ;
#9137 = CARTESIAN_POINT ( 'NONE',  ( -1.461580736456472351, -1.461580736456473018, -1.849999998907525534 ) ) ;
#9138 = CARTESIAN_POINT ( 'NONE',  ( 1.035533905932737975, 185.7500000000000568, 4.500000000000000888 ) ) ;
#9139 = CARTESIAN_POINT ( 'NONE',  ( -2.500000000000000444, 184.0000000000000000, 7.000000000000000000 ) ) ;
#9140 = EDGE_CURVE ( 'NONE', #3737, #9045, #12327, .T. ) ;
#9142 = VERTEX_POINT ( 'NONE', #12807 ) ;
#9141 = CARTESIAN_POINT ( 'NONE',  ( -0.6144377077727894987, -5.969178481556086879, 23.70033966857735663 ) ) ;
#9143 = DIRECTION ( 'NONE',  ( -0.5877852522924685852, -0.8090169943749508930, 0.000000000000000000 ) ) ;
#9144 = CARTESIAN_POINT ( 'NONE',  ( -0.9999171162589696182, -6.169494774098548184, 4.867223203306743073 ) ) ;
#9145 = CARTESIAN_POINT ( 'NONE',  ( -0.0003580824083057882324, 226.3251816641676726, 4.486670979270475534 ) ) ;
#9146 = DIRECTION ( 'NONE',  ( 0.000000000000000000, 0.000000000000000000, 1.000000000000000000 ) ) ;
#9147 = CARTESIAN_POINT ( 'NONE',  ( 2.491866682565489377, 188.9999999978042524, 7.260727731289393638 ) ) ;
#9148 = DIRECTION ( 'NONE',  ( 0.8090169943749506709, -0.5877852522924686962, 0.000000000000000000 ) ) ;
#9149 = CARTESIAN_POINT ( 'NONE',  ( -5.329907877631355539, -2.755840666746254275, 5.261943240031468072 ) ) ;
#9150 = CARTESIAN_POINT ( 'NONE',  ( 1.496490727326450720, 228.6905582067893477, 8.233762344832721070 ) ) ;
#9151 = CARTESIAN_POINT ( 'NONE',  ( 5.726049995854543440, -2.506679546901704470, 23.70045537531157365 ) ) ;
#9152 = CARTESIAN_POINT ( 'NONE',  ( -5.770167736194727226, 2.404664418229086831, 4.126326713640078303 ) ) ;
#9153 = CARTESIAN_POINT ( 'NONE',  ( -4.286401442266546624, -4.198423832313178394, 31.00000000000000000 ) ) ;
#9154 = EDGE_LOOP ( 'NONE', ( #2171, #12753 ) ) ;
#9155 = CARTESIAN_POINT ( 'NONE',  ( 2.066987300000000083, 186.5999999989074922, 7.856174172912946396 ) ) ;
#9156 = DIRECTION ( 'NONE',  ( 0.000000000000000000, 0.000000000000000000, 1.000000000000000000 ) ) ;
#9157 = STYLED_ITEM ( 'NONE', ( #14698 ), #12380 ) ;
#9158 = ORIENTED_EDGE ( 'NONE', *, *, #14246, .T. ) ;
#9159 = EDGE_CURVE ( 'NONE', #15176, #14218, #3224, .T. ) ;
#9160 = FACE_OUTER_BOUND ( 'NONE', #15114, .T. ) ;
#9161 = LINE ( 'NONE', #10425, #5644 ) ;
#9162 = CARTESIAN_POINT ( 'NONE',  ( -2.500000000000000444, 1.035533905932737753, -1.549999999999999822 ) ) ;
#9163 = CARTESIAN_POINT ( 'NONE',  ( 0.8561741729129458411, 184.3999999989075320, 4.933012699999999029 ) ) ;
#9164 = CARTESIAN_POINT ( 'NONE',  ( 5.487097279078525958, -2.429065649168602015, 23.70047945897283270 ) ) ;
#9165 = CARTESIAN_POINT ( 'NONE',  ( 2.500000000000000444, -1.035533905932737309, -1.150000000000000133 ) ) ;
#9166 = CARTESIAN_POINT ( 'NONE',  ( -2.500000000000000000, -1.035533905932739307, -1.450000000000000400 ) ) ;
#9167 = CARTESIAN_POINT ( 'NONE',  ( 0.000000000000000000, 215.7452399395091049, 13.29567785264566027 ) ) ;
#9168 = DIRECTION ( 'NONE',  ( 0.000000000000000000, 0.000000000000000000, -1.000000000000000000 ) ) ;
#9169 = LINE ( 'NONE', #10663, #413 ) ;
#9170 = CARTESIAN_POINT ( 'NONE',  ( -0.7993401192311766490, 6.199366368793662652, 31.61483246936573011 ) ) ;
#9171 = ORIENTED_EDGE ( 'NONE', *, *, #13177, .T. ) ;
#9172 = ORIENTED_EDGE ( 'NONE', *, *, #2098, .T. ) ;
#9173 = EDGE_LOOP ( 'NONE', ( #7503, #4835 ) ) ;
#9174 = CARTESIAN_POINT ( 'NONE',  ( 3.882809187878950574, -4.899079348630037245, 12.47400098023328674 ) ) ;
#9175 = CARTESIAN_POINT ( 'NONE',  ( -2.668367453516691690, -5.373994336898102020, 11.49999999999998224 ) ) ;
#9176 = ORIENTED_EDGE ( 'NONE', *, *, #7457, .F. ) ;
#9177 = FACE_OUTER_BOUND ( 'NONE', #10437, .T. ) ;
#9178 = CARTESIAN_POINT ( 'NONE',  ( -1.035533905932737753, 2.500000000000000444, 0.05000000218494961984 ) ) ;
#9179 = CARTESIAN_POINT ( 'NONE',  ( 5.558508435838239059, -2.857531096718835428, 31.00000000000000000 ) ) ;
#9180 = CARTESIAN_POINT ( 'NONE',  ( 2.030576276931546336E-13, -6.250000000000000888, 25.49999999999999645 ) ) ;
#9181 = CARTESIAN_POINT ( 'NONE',  ( 1.767766952966368432, 187.7999999978150356, 8.767766952966368876 ) ) ;
#9182 = CARTESIAN_POINT ( 'NONE',  ( 9.825582188149883933E-17, 184.8999999978150584, 4.500000000000000000 ) ) ;
#9183 = CARTESIAN_POINT ( 'NONE',  ( 5.931793676715101604, 0.9035324301688090198, 18.26239891805595050 ) ) ;
#9184 = SHAPE_DEFINITION_REPRESENTATION ( #15297, #11283 ) ;
#9185 = CARTESIAN_POINT ( 'NONE',  ( -1.461580736456472795, 1.461580736456472795, 1.950000001092474733 ) ) ;
#9186 = CARTESIAN_POINT ( 'NONE',  ( -1.016439536705160407E-16, 188.1699999975965625, 4.500000000000000000 ) ) ;
#9187 = CARTESIAN_POINT ( 'NONE',  ( 1.583222688839772019, 228.1098062731747689, 9.740983991995673108 ) ) ;
#9188 = CARTESIAN_POINT ( 'NONE',  ( 3.883716939928966383, 4.898343590941268033, 18.97359571723300675 ) ) ;
#9189 = ORIENTED_EDGE ( 'NONE', *, *, #1274, .T. ) ;
#9190 = CARTESIAN_POINT ( 'NONE',  ( 1.965078059614901340, 1.570455839174875301, -2.498889909998655678 ) ) ;
#9191 = ORIENTED_EDGE ( 'NONE', *, *, #4080, .F. ) ;
#9192 = CARTESIAN_POINT ( 'NONE',  ( 4.069800786343853893, -4.744882212776776242, 5.873819640450717472 ) ) ;
#9193 = CARTESIAN_POINT ( 'NONE',  ( -5.558508435838188433, -2.857531096718932684, 5.000000000000004441 ) ) ;
#9194 = CARTESIAN_POINT ( 'NONE',  ( -1.000049560716552044, 5.916071405810145123, 4.869677990115311772 ) ) ;
#9195 = ORIENTED_EDGE ( 'NONE', *, *, #4632, .F. ) ;
#9196 = DIRECTION ( 'NONE',  ( -0.5877852522924685852, -0.8090169943749508930, 0.000000000000000000 ) ) ;
#9197 = CARTESIAN_POINT ( 'NONE',  ( -0.8738239080078270549, -6.188820299975621886, 25.00355795710143170 ) ) ;
#9198 = FILL_AREA_STYLE ('',( #7918 ) ) ;
#9199 = CARTESIAN_POINT ( 'NONE',  ( -1.530808498934191571E-16, 2.500000000000000000, -0.9000000000000002442 ) ) ;
#9200 = CARTESIAN_POINT ( 'NONE',  ( -8.250000000000003553, 3.401296724241641415E-14, 2.000000000000001776 ) ) ;
#9201 = CARTESIAN_POINT ( 'NONE',  ( -1.035533905932737753, 2.500000000000000444, 1.650000002184949910 ) ) ;
#9202 = PRODUCT_DEFINITION_SHAPE ( 'NONE', 'NONE',  #15757 ) ;
#9203 = CARTESIAN_POINT ( 'NONE',  ( -1.767766952966369098, 184.9999999978150527, 5.232233047033630235 ) ) ;
#9204 = ADVANCED_FACE ( 'NONE', ( #5744 ), #11619, .F. ) ;
#9205 = CARTESIAN_POINT ( 'NONE',  ( 0.3900692251286368428, 228.2474522196246767, 10.14569219465573546 ) ) ;
#9206 = FACE_BOUND ( 'NONE', #14900, .T. ) ;
#9207 = EDGE_CURVE ( 'NONE', #12866, #4157, #11773, .T. ) ;
#9208 = B_SPLINE_CURVE_WITH_KNOTS ( 'NONE', 3,
 ( #6954, #11787, #3355, #888, #8223, #13058, #13138, #7030, #11858, #14324, #3431, #7109, #5913, #10761, #12341, #14412, #1362, #12103 ),
 .UNSPECIFIED., .F., .F.,
 ( 4, 2, 2, 2, 2, 2, 2, 2, 4 ),
 ( 0.003131486019301987257, 0.003522824630466693530, 0.003914163241631399802, 0.004305501852796106074, 0.004696840463960812347, 0.005088179075125518619, 0.005479517686290224891, 0.005870856297454931164, 0.006262194908619637436 ),
 .UNSPECIFIED. ) ;
#9209 = CARTESIAN_POINT ( 'NONE',  ( -5.746996058422752185, 1.729015645941996304, 19.00007961174475568 ) ) ;
#9210 = CARTESIAN_POINT ( 'NONE',  ( -0.8561741729129458411, -2.066987299999999195, -2.599999998907525534 ) ) ;
#9211 = VECTOR ( 'NONE', #6585, 1000.000000000000000 ) ;
#9212 = CARTESIAN_POINT ( 'NONE',  ( -1.767766952966369765, 186.0999999999999943, 8.767766952966368876 ) ) ;
#9213 = CARTESIAN_POINT ( 'NONE',  ( 3.882809187878850654, -4.899079348630117181, 25.47400098023329917 ) ) ;
#9215 = VERTEX_POINT ( 'NONE', #5589 ) ;
#9214 = LINE ( 'NONE', #768, #13350 ) ;
#9216 = CARTESIAN_POINT ( 'NONE',  ( 7.180990026460803755, -3.384707322287205944, 24.49999999999999289 ) ) ;
#9217 = CARTESIAN_POINT ( 'NONE',  ( -2.500000000000000444, 186.7500000000000000, 5.964466094067261359 ) ) ;
#9218 = CARTESIAN_POINT ( 'NONE',  ( -1.016439536705160407E-17, 228.2551366889529731, 10.16828399152529272 ) ) ;
#9219 = ADVANCED_FACE ( 'NONE', ( #10436 ), #13121, .F. ) ;
#9220 = DIRECTION ( 'NONE',  ( -0.3090169943749447867, -0.9510565162951544194, 0.000000000000000000 ) ) ;
#9221 = AXIS2_PLACEMENT_3D ( 'NONE', #13460, #7420, #4880 ) ;
#9222 = CARTESIAN_POINT ( 'NONE',  ( 0.08612881260894005020, 189.4418673018899142, 3.980892592272581076 ) ) ;
#9223 = CARTESIAN_POINT ( 'NONE',  ( -1.035533905932737975, 185.7800000002185072, 4.500000000000000888 ) ) ;
#9224 = CARTESIAN_POINT ( 'NONE',  ( 0.000000000000000000, 0.000000000000000000, 2.000000000000001776 ) ) ;
#9225 = CARTESIAN_POINT ( 'NONE',  ( 0.7014106675288342974, 228.8704641679326244, 8.753341021778663134 ) ) ;
#9226 = CARTESIAN_POINT ( 'NONE',  ( 5.903596343266283242, 2.055998103990630099, 10.50004921015705150 ) ) ;
#9227 = CARTESIAN_POINT ( 'NONE',  ( -5.984595133899197172, 1.806709459528603956, 4.000049210157070156 ) ) ;
#9228 = LINE ( 'NONE', #3399, #13044 ) ;
#9229 = ORIENTED_EDGE ( 'NONE', *, *, #15431, .F. ) ;
#9230 = CARTESIAN_POINT ( 'NONE',  ( 0.000000000000000000, 186.0499999989075093, 4.933012699999999029 ) ) ;
#9231 = CARTESIAN_POINT ( 'NONE',  ( -4.435347140101058017, -4.403429997944488861, 11.63060690723496293 ) ) ;
#9232 = ORIENTED_EDGE ( 'NONE', *, *, #11062, .T. ) ;
#9233 = DIRECTION ( 'NONE',  ( -0.000000000000000000, 1.000000000000000000, -0.000000000000000000 ) ) ;
#9234 = CARTESIAN_POINT ( 'NONE',  ( -1.265664690411614835E-16, 2.066987299999999639, -2.949999998907525178 ) ) ;
#9235 = CARTESIAN_POINT ( 'NONE',  ( 8.809142651444723526E-17, 184.6499999989075320, 4.933012699999999029 ) ) ;
#9236 = CARTESIAN_POINT ( 'NONE',  ( 2.500000000000000444, 184.0000000000000000, 7.000000000000000000 ) ) ;
#9237 = CARTESIAN_POINT ( 'NONE',  ( -4.302927372051845722E-16, 184.8499999989074922, 9.066987300000000971 ) ) ;
#9238 = CARTESIAN_POINT ( 'NONE',  ( 3.061616997868383141E-16, 0.000000000000000000, 2.500000000000000000 ) ) ;
#9239 = CARTESIAN_POINT ( 'NONE',  ( 1.035533905932739085, -2.500000000000000000, 0.4500000021849498988 ) ) ;
#9240 = DIRECTION ( 'NONE',  ( 0.000000000000000000, -1.000000000000000000, 0.000000000000000000 ) ) ;
#9241 = CARTESIAN_POINT ( 'NONE',  ( 0.000000000000000000, 194.5935680195190116, 12.11154058223188201 ) ) ;
#9242 = CARTESIAN_POINT ( 'NONE',  ( -5.746996058422731757, -1.729015645942072688, 16.99992038825522656 ) ) ;
#9243 = ADVANCED_FACE ( 'NONE', ( #9245, #2067 ), #11844, .F. ) ;
#9244 = AXIS2_PLACEMENT_3D ( 'NONE', #9360, #14199, #1952 ) ;
#9245 = FACE_OUTER_BOUND ( 'NONE', #3505, .T. ) ;
#9246 = VERTEX_POINT ( 'NONE', #10585 ) ;
#9247 = VERTEX_POINT ( 'NONE', #6940 ) ;
#9248 = EDGE_CURVE ( 'NONE', #6928, #9324, #6449, .T. ) ;
#9249 = ORIENTED_EDGE ( 'NONE', *, *, #8279, .T. ) ;
#9250 = CARTESIAN_POINT ( 'NONE',  ( 3.419318284370132410, -4.932111238568221978, 25.49992002356261622 ) ) ;
#9251 = CARTESIAN_POINT ( 'NONE',  ( 2.030576276931546336E-13, -6.000000000000000888, 25.49999999999999645 ) ) ;
#9252 = ORIENTED_EDGE ( 'NONE', *, *, #10963, .F. ) ;
#9253 = CARTESIAN_POINT ( 'NONE',  ( 1.767766952966369320, 184.9000000000000057, 5.232233047033630235 ) ) ;
#9254 = CARTESIAN_POINT ( 'NONE',  ( 4.592425496802573972E-16, -2.500000000000000000, 1.200000002184949510 ) ) ;
#9255 = CARTESIAN_POINT ( 'NONE',  ( -5.329907877631348434, -2.755840666746270262, 31.26194324003147429 ) ) ;
#9256 = CARTESIAN_POINT ( 'NONE',  ( -3.255128505894222535, -5.336774832660773349, 4.126199447526042619 ) ) ;
#9257 = CARTESIAN_POINT ( 'NONE',  ( -7.352245982167326943E-16, 188.4999999978150527, 9.500000000000001776 ) ) ;
#9258 = CARTESIAN_POINT ( 'NONE',  ( -2.499999999999999556, 185.0499999978150072, 5.964466094067259583 ) ) ;
#9259 = CARTESIAN_POINT ( 'NONE',  ( -4.000000000000001776, 184.0000000000000000, 7.000000000000000888 ) ) ;
#9260 = APPLICATION_PROTOCOL_DEFINITION ( 'draft international standard', 'automotive_design', 1998, #9645 ) ;
#9261 = CARTESIAN_POINT ( 'NONE',  ( 2.066987299999999639, 2.531329380823229670E-16, 0.05000000109247476621 ) ) ;
#9262 = EDGE_CURVE ( 'NONE', #13656, #13850, #14987, .T. ) ;
#9263 = CARTESIAN_POINT ( 'NONE',  ( -5.935543223013848291, -0.8771126767607491104, 4.867639214160894845 ) ) ;
#9264 = CARTESIAN_POINT ( 'NONE',  ( 1.628454131612142364, 226.4793820939146372, 4.941229787183066158 ) ) ;
#9265 = DIRECTION ( 'NONE',  ( 0.8090169943749506709, -0.5877852522924686962, 0.000000000000000000 ) ) ;
#9266 = EDGE_LOOP ( 'NONE', ( #5593, #5402, #9520, #12569 ) ) ;
#9267 = CARTESIAN_POINT ( 'NONE',  ( -2.432277057295939571, -0.6446960933136758332, -2.500850192709198616 ) ) ;
#9268 = EDGE_LOOP ( 'NONE', ( #1919, #11079 ) ) ;
#9269 = CARTESIAN_POINT ( 'NONE',  ( 6.780834061396424457E-14, 6.250000000000000888, 10.49999999999998224 ) ) ;
#9270 = VECTOR ( 'NONE', #4725, 1000.000000000000000 ) ;
#9271 = CARTESIAN_POINT ( 'NONE',  ( 6.176542424588121527, -0.9554180641285238140, 31.00000000000000000 ) ) ;
#9272 = CARTESIAN_POINT ( 'NONE',  ( 5.770331821586450971, 2.404225004693483658, 23.62619944752604439 ) ) ;
#9273 = ORIENTED_EDGE ( 'NONE', *, *, #10171, .T. ) ;
#9274 = CARTESIAN_POINT ( 'NONE',  ( 0.000000000000000000, 184.0000000000000000, 7.000000000000000000 ) ) ;
#9275 = FACE_BOUND ( 'NONE', #4094, .T. ) ;
#9276 = CARTESIAN_POINT ( 'NONE',  ( 4.592425496802573972E-16, -2.500000000000000000, 1.899999999999999911 ) ) ;
#9277 = CARTESIAN_POINT ( 'NONE',  ( 2.500000000000000000, 3.061616997868383141E-16, -1.100000000000000311 ) ) ;
#9278 = CARTESIAN_POINT ( 'NONE',  ( -3.883588957979317247, -4.898466244118881541, 25.47377282875268278 ) ) ;
#9279 = FILL_AREA_STYLE_COLOUR ( '', #1768 ) ;
#9280 = DIRECTION ( 'NONE',  ( 0.000000000000000000, 0.000000000000000000, 1.000000000000000000 ) ) ;
#9281 = CARTESIAN_POINT ( 'NONE',  ( 2.500000000000000444, 184.6999999978150697, 7.000000000000000000 ) ) ;
#9282 = EDGE_CURVE ( 'NONE', #3268, #14489, #10810, .T. ) ;
#9283 = CARTESIAN_POINT ( 'NONE',  ( -1.770887355114397321, 228.5581793045761287, 7.851444524843710582 ) ) ;
#9284 = FACE_BOUND ( 'NONE', #6533, .T. ) ;
#9285 = CARTESIAN_POINT ( 'NONE',  ( -5.317509234263907203, 2.779225709351096363, 18.13061695532137207 ) ) ;
#9286 = CARTESIAN_POINT ( 'NONE',  ( -2.066987299999999639, 0.000000000000000000, -1.949999998907525178 ) ) ;
#9287 = CARTESIAN_POINT ( 'NONE',  ( -1.035533905932737975, 186.6500000000000057, 4.500000000000000888 ) ) ;
#9288 = DIRECTION ( 'NONE',  ( -1.062480551894329776E-17, -2.775557561562888393E-16, 1.000000000000000000 ) ) ;
#9290 = VERTEX_POINT ( 'NONE', #238 ) ;
#9289 = FACE_OUTER_BOUND ( 'NONE', #12966, .T. ) ;
#9291 = CARTESIAN_POINT ( 'NONE',  ( -5.558508435838167117, 2.857531096718976205, 18.13060690723497004 ) ) ;
#9292 = CARTESIAN_POINT ( 'NONE',  ( -0.0007161861819565282445, 226.3251816840472657, 4.486671040222605988 ) ) ;
#9293 = CARTESIAN_POINT ( 'NONE',  ( -2.048913241472479108, 189.7603925237210660, 9.570315070074567387 ) ) ;
#9294 = CARTESIAN_POINT ( 'NONE',  ( 1.500000000000000000, 9.750000000000003553, 0.000000000000000000 ) ) ;
#9295 = CARTESIAN_POINT ( 'NONE',  ( -1.035533905932737753, 184.1800000002185129, 4.500000000000000888 ) ) ;
#9296 = CARTESIAN_POINT ( 'NONE',  ( -1.990566740715900895, 228.1747751937680846, 6.744151584892693840 ) ) ;
#9297 = CARTESIAN_POINT ( 'NONE',  ( 1.984153134209927671, 228.3142122347729526, 7.146853712282291049 ) ) ;
#9298 = FACE_BOUND ( 'NONE', #4056, .T. ) ;
#9299 = DIRECTION ( 'NONE',  ( 0.000000000000000000, 0.000000000000000000, -1.000000000000000000 ) ) ;
#9300 = CARTESIAN_POINT ( 'NONE',  ( 0.2624013748573350013, 5.995472630654520074, 30.02628559691082444 ) ) ;
#9301 = AXIS2_PLACEMENT_3D ( 'NONE', #2113, #3314, #5711 ) ;
#9302 = VERTEX_POINT ( 'NONE', #7331 ) ;
#9303 = CARTESIAN_POINT ( 'NONE',  ( 9.825582188149883933E-17, 184.4499999989075150, 4.933012699999999029 ) ) ;
#9304 = CARTESIAN_POINT ( 'NONE',  ( -1.767766952966369542, 184.5000000000000000, 8.767766952966368876 ) ) ;
#9305 = EDGE_CURVE ( 'NONE', #12468, #14260, #15054, .T. ) ;
#9306 = ORIENTED_EDGE ( 'NONE', *, *, #15588, .F. ) ;
#9307 = EDGE_CURVE ( 'NONE', #7142, #15044, #5100, .T. ) ;
#9308 = CARTESIAN_POINT ( 'NONE',  ( -2.500000000000000444, 186.0499999999999829, 8.035533905932737753 ) ) ;
#9309 = CARTESIAN_POINT ( 'NONE',  ( 1.767766952966368654, 1.767766952966369098, -0.09999999781505011787 ) ) ;
#9310 = CARTESIAN_POINT ( 'NONE',  ( 4.069800786343690469, 4.744882212776914798, 17.12618035954927720 ) ) ;
#9311 = CARTESIAN_POINT ( 'NONE',  ( -2.066987300000000971, 186.2999999989075093, 7.856174172912944620 ) ) ;
#9312 = CARTESIAN_POINT ( 'NONE',  ( -4.435347140101010055, -4.403429997944535046, 5.000000000000004441 ) ) ;
#9313 = CARTESIAN_POINT ( 'NONE',  ( 2.500000000000000444, 1.035533905932737975, -0.1499999978150502733 ) ) ;
#9314 = CARTESIAN_POINT ( 'NONE',  ( 4.142173849413770981, -4.341773579105383085, 10.88480617551147134 ) ) ;
#9315 = CARTESIAN_POINT ( 'NONE',  ( -5.999999999999999112, 202.3202208672780102, 7.308763624254441815 ) ) ;
#9316 = CARTESIAN_POINT ( 'NONE',  ( 5.317509234263932072, 2.779225709351047957, 5.000000000000004441 ) ) ;
#9317 = CARTESIAN_POINT ( 'NONE',  ( -5.375605342016431365, -2.665598297262440131, 17.49687951097621763 ) ) ;
#9318 = CARTESIAN_POINT ( 'NONE',  ( 5.903230462362958342, 1.077253041748864604, 12.11442521571935949 ) ) ;
#9319 = ORIENTED_EDGE ( 'NONE', *, *, #11630, .F. ) ;
#9320 = ORIENTED_EDGE ( 'NONE', *, *, #9950, .T. ) ;
#9321 = ORIENTED_EDGE ( 'NONE', *, *, #9761, .F. ) ;
#9322 = CARTESIAN_POINT ( 'NONE',  ( 9.750000000000003553, 182.0000000000000000, 1.020968533498575461E-13 ) ) ;
#9323 = CARTESIAN_POINT ( 'NONE',  ( 0.6427959281715842632, 227.6423845907872021, 5.206577157913290677 ) ) ;
#9324 = VERTEX_POINT ( 'NONE', #7174 ) ;
#9325 = PRODUCT_DEFINITION_SHAPE ( 'NONE', 'NONE',  #15733 ) ;
#9326 = CARTESIAN_POINT ( 'NONE',  ( 2.500000000000000000, 3.061616997868383141E-16, 1.400000002184949688 ) ) ;
#9327 = CARTESIAN_POINT ( 'NONE',  ( -5.375763363753427448, -2.665284979407579691, 31.50389795015983552 ) ) ;
#9328 = DIRECTION ( 'NONE',  ( -1.000000000000000000, 0.000000000000000000, 0.000000000000000000 ) ) ;
#9329 = CARTESIAN_POINT ( 'NONE',  ( -1.035533905932739751, 188.4499999978150413, 9.500000000000003553 ) ) ;
#9330 = CARTESIAN_POINT ( 'NONE',  ( 1.767766952966368654, 1.767766952966369098, -0.9930000000218494050 ) ) ;
#9331 = AXIS2_PLACEMENT_3D ( 'NONE', #1561, #7533, #1398 ) ;
#9332 = CARTESIAN_POINT ( 'NONE',  ( 4.743384504624081899E-17, 185.6999999978150697, 4.500000000000000000 ) ) ;
#9333 = CONTEXT_DEPENDENT_SHAPE_REPRESENTATION ( #12872, #3617 ) ;
#9334 = CARTESIAN_POINT ( 'NONE',  ( -1.461580736456472795, 1.461580736456472795, 1.150000001092474688 ) ) ;
#9335 = CARTESIAN_POINT ( 'NONE',  ( -5.866923913994641637, -1.260079467906541684, 4.200479458972859348 ) ) ;
#9336 = CARTESIAN_POINT ( 'NONE',  ( 2.976061188595913176, 227.1638826975962502, 6.957706536906315797 ) ) ;
#9337 = CARTESIAN_POINT ( 'NONE',  ( -1.328763708711319325, 228.1557872355912195, 9.876186263205003257 ) ) ;
#9338 = ADVANCED_FACE ( 'NONE', ( #11058 ), #2304, .F. ) ;
#9339 = VERTEX_POINT ( 'NONE', #14803 ) ;
#9340 = CARTESIAN_POINT ( 'NONE',  ( 2.500000000000000000, 188.6499999978150584, 8.035533905932739529 ) ) ;
#9341 = AXIS2_PLACEMENT_3D ( 'NONE', #2823, #7748, #7671 ) ;
#9342 = EDGE_LOOP ( 'NONE', ( #2905, #1191, #15290, #14530 ) ) ;
#9343 = CARTESIAN_POINT ( 'NONE',  ( 4.344265632482186668, -4.493596842504861577, 5.504259495030091820 ) ) ;
#9344 = CARTESIAN_POINT ( 'NONE',  ( 4.286401442266496886, -4.198423832313229020, 17.86760611998365178 ) ) ;
#9345 = CARTESIAN_POINT ( 'NONE',  ( 6.172651332693114057, 0.9815532474592564283, 24.23809786915987985 ) ) ;
#9346 = EDGE_CURVE ( 'NONE', #10381, #546, #3389, .T. ) ;
#9347 = ORIENTED_EDGE ( 'NONE', *, *, #4264, .F. ) ;
#9348 = CARTESIAN_POINT ( 'NONE',  ( -5.746837578675986435, 1.729433780394314502, 17.00004946353775992 ) ) ;
#9349 = FACE_BOUND ( 'NONE', #14587, .T. ) ;
#9350 = DIRECTION ( 'NONE',  ( -1.000000000000000000, 0.000000000000000000, 0.000000000000000000 ) ) ;
#9351 = CARTESIAN_POINT ( 'NONE',  ( 1.035533905932739085, -2.500000000000000000, -2.049999999999999822 ) ) ;
#9352 = CARTESIAN_POINT ( 'NONE',  ( -2.841519077896259127, -5.566940434249956660, 24.76379616840806008 ) ) ;
#9353 = VECTOR ( 'NONE', #4729, 1000.000000000000114 ) ;
#9354 = CARTESIAN_POINT ( 'NONE',  ( 0.09128442572522987852, 0.4000000000000062395, -2.551849451881606168 ) ) ;
#9355 = CARTESIAN_POINT ( 'NONE',  ( 1.035533905932737753, 188.9499999999999886, 4.500000000000000888 ) ) ;
#9356 = CIRCLE ( 'NONE', #2497, 2.499999999999999556 ) ;
#9357 = CARTESIAN_POINT ( 'NONE',  ( -6.020865209844600052, 1.681180471732123483, 12.47400098023328674 ) ) ;
#9358 = CARTESIAN_POINT ( 'NONE',  ( -0.7013870287959992345, 228.8704690996177646, 8.753355264767147759 ) ) ;
#9359 = FACE_BOUND ( 'NONE', #8415, .T. ) ;
#9360 = CARTESIAN_POINT ( 'NONE',  ( -13.50000000000000000, 2.000000000000000000, 2.479909768273400161E-15 ) ) ;
#9361 = CARTESIAN_POINT ( 'NONE',  ( -1.461580736456472795, 1.461580736456472795, -2.049999998907525711 ) ) ;
#9362 = CARTESIAN_POINT ( 'NONE',  ( 1.767766952966368432, 187.0999999999999943, 8.767766952966368876 ) ) ;
#9363 = CARTESIAN_POINT ( 'NONE',  ( 3.566234721237978356, -5.134387337253871308, 25.49991741810288559 ) ) ;
#9364 = AXIS2_PLACEMENT_3D ( 'NONE', #12737, #14012, #15138 ) ;
#9366 = ORIENTED_EDGE ( 'NONE', *, *, #7892, .F. ) ;
#9365 = CARTESIAN_POINT ( 'NONE',  ( -0.9737778612003452627, -5.920671847850547564, 24.23736375884649519 ) ) ;
#9367 = CIRCLE ( 'NONE', #1736, 1.499999999999999556 ) ;
#9368 = DIRECTION ( 'NONE',  ( 0.5877852522924802425, -0.8090169943749422332, 0.000000000000000000 ) ) ;
#9369 = CIRCLE ( 'NONE', #8872, 1.999999999999999556 ) ;
#9370 = CARTESIAN_POINT ( 'NONE',  ( -2.066987299999999639, 0.000000000000000000, 2.250000001092474999 ) ) ;
#9371 = CARTESIAN_POINT ( 'NONE',  ( -2.684371489741315120, 227.7208608295982799, 8.597006646416071263 ) ) ;
#9372 =( LENGTH_UNIT ( ) NAMED_UNIT ( * ) SI_UNIT ( .MILLI., .METRE. ) );
#9373 = CARTESIAN_POINT ( 'NONE',  ( 6.106056299406772858, 1.336851112280557974, 25.29887838423337953 ) ) ;
#9374 = CYLINDRICAL_SURFACE ( 'NONE', #4796, 1.000000000000000222 ) ;
#9375 = CARTESIAN_POINT ( 'NONE',  ( -4.435347140101074004, 4.403429997944469321, 5.000000000000004441 ) ) ;
#9376 = CARTESIAN_POINT ( 'NONE',  ( 1.452733574390970395, 228.7063250495755540, 8.279297886081021574 ) ) ;
#9377 = FACE_BOUND ( 'NONE', #10969, .T. ) ;
#9378 = LINE ( 'NONE', #15266, #164 ) ;
#9379 = CARTESIAN_POINT ( 'NONE',  ( -4.196038884587139250, -4.289036423669302600, 30.49610204984016448 ) ) ;
#9380 = ORIENTED_EDGE ( 'NONE', *, *, #9594, .T. ) ;
#9381 = CARTESIAN_POINT ( 'NONE',  ( -2.066987300000000971, 184.5999999989074922, 6.143825827087054492 ) ) ;
#9382 = CARTESIAN_POINT ( 'NONE',  ( 2.782156709077397760, 5.316215864844059169, 30.49687951097622118 ) ) ;
#9383 = EDGE_LOOP ( 'NONE', ( #9895, #11649 ) ) ;
#9384 = FACE_OUTER_BOUND ( 'NONE', #4832, .T. ) ;
#9385 = VECTOR ( 'NONE', #5809, 1000.000000000000000 ) ;
#9386 = CARTESIAN_POINT ( 'NONE',  ( 2.066987300000000083, 184.4999999989074979, 6.143825827087054492 ) ) ;
#9387 = CARTESIAN_POINT ( 'NONE',  ( 4.435347140100915908, 4.403429997944633634, 17.86765874365829276 ) ) ;
#9388 = CARTESIAN_POINT ( 'NONE',  ( 2.066987300000000083, 186.5999999989074922, 7.856174172912946396 ) ) ;
#9389 = DIRECTION ( 'NONE',  ( -0.000000000000000000, -1.000000000000000000, -0.000000000000000000 ) ) ;
#9390 = CARTESIAN_POINT ( 'NONE',  ( -2.500000000000000000, -1.035533905932739307, -1.349999997815050090 ) ) ;
#9391 = FACE_OUTER_BOUND ( 'NONE', #14905, .T. ) ;
#9392 = CARTESIAN_POINT ( 'NONE',  ( -5.999999999999999112, 215.0542865858234336, 7.296348638347391891 ) ) ;
#9393 = CARTESIAN_POINT ( 'NONE',  ( -1.035533905932737753, 2.500000000000000444, 0.7499999999999998890 ) ) ;
#9394 = CARTESIAN_POINT ( 'NONE',  ( -2.066987299999999195, -0.8561741729129466183, -2.499999998907525001 ) ) ;
#9395 = CARTESIAN_POINT ( 'NONE',  ( 5.915755444410801367, 1.003187219519861895, 12.00312048902374862 ) ) ;
#9396 = EDGE_CURVE ( 'NONE', #7094, #10183, #4358, .T. ) ;
#9397 = ORIENTED_EDGE ( 'NONE', *, *, #12918, .T. ) ;
#9398 = COLOUR_RGB ( '', 0.09019608, 0.27058824, 0.51372549) ;
#9399 = ORIENTED_EDGE ( 'NONE', *, *, #14160, .F. ) ;
#9400 = ORIENTED_EDGE ( 'NONE', *, *, #13572, .F. ) ;
#9401 = CARTESIAN_POINT ( 'NONE',  ( 2.066987300000000083, 184.4499999989075150, 7.000000000000000000 ) ) ;
#9402 = CARTESIAN_POINT ( 'NONE',  ( -3.735642931251092591, 4.696778275484423837, 12.47408052783099031 ) ) ;
#9403 = ORIENTED_EDGE ( 'NONE', *, *, #8486, .T. ) ;
#9404 = CARTESIAN_POINT ( 'NONE',  ( 2.066987299999999639, 2.531329380823229670E-16, 1.650000001092474911 ) ) ;
#9405 = EDGE_CURVE ( 'NONE', #14984, #11235, #11366, .T. ) ;
#9406 = CARTESIAN_POINT ( 'NONE',  ( -1.000049560716352426, 5.916071405810178874, 24.36967799011533131 ) ) ;
#9407 = DIRECTION ( 'NONE',  ( 0.000000000000000000, 1.000000000000000000, 0.000000000000000000 ) ) ;
#9408 = CARTESIAN_POINT ( 'NONE',  ( 2.500000000000000444, 187.8499999978150470, 8.035533905932739529 ) ) ;
#9409 = CARTESIAN_POINT ( 'NONE',  ( 4.592425496802573972E-16, -2.500000000000000000, 0.3069999999781504174 ) ) ;
#9410 = B_SPLINE_CURVE_WITH_KNOTS ( 'NONE', 3,
 ( #2501, #1142, #11010, #6172, #2417, #108, #15633, #5929, #7043, #986, #3687, #7357, #4976, #7204, #7283, #14428, #9753, #3532 ),
 .UNSPECIFIED., .F., .F.,
 ( 4, 2, 2, 2, 2, 2, 2, 2, 4 ),
 ( 0.003131918686235973890, 0.003523310662250265894, 0.003914702638264557465, 0.004306094614278849902, 0.004697486590293141473, 0.005088878566307433043, 0.005480270542321723747, 0.005871662518336014450, 0.006263054494350305153 ),
 .UNSPECIFIED. ) ;
#9411 = CARTESIAN_POINT ( 'NONE',  ( 1.035533905932737975, 185.6499999978150584, 4.500000000000001776 ) ) ;
#9412 = EDGE_CURVE ( 'NONE', #9005, #7444, #2062, .T. ) ;
#9413 = CONTEXT_DEPENDENT_SHAPE_REPRESENTATION ( #3727, #10593 ) ;
#9414 = CARTESIAN_POINT ( 'NONE',  ( 1.461580736456473018, -1.461580736456472573, -0.04999999890752549608 ) ) ;
#9415 = CARTESIAN_POINT ( 'NONE',  ( 1.767766952966369098, 188.8699999975965511, 5.232233047033630235 ) ) ;
#9416 = CARTESIAN_POINT ( 'NONE',  ( 2.548737910730607403, 227.7996913757372397, 8.828908791204545636 ) ) ;
#9417 = CARTESIAN_POINT ( 'NONE',  ( 4.435347140100914132, 4.403429997944631857, 17.99999999999998934 ) ) ;
#9418 = ORIENTED_EDGE ( 'NONE', *, *, #15326, .F. ) ;
#9419 = CARTESIAN_POINT ( 'NONE',  ( -5.409007216690624453, 2.598315788643851043, 25.11442521571937547 ) ) ;
#9420 = ORIENTED_EDGE ( 'NONE', *, *, #15100, .T. ) ;
#9421 = ORIENTED_EDGE ( 'NONE', *, *, #4590, .F. ) ;
#9422 = CARTESIAN_POINT ( 'NONE',  ( 0.9999171162589906015, 6.169494774098545520, 30.86722320330672531 ) ) ;
#9423 = PRESENTATION_STYLE_ASSIGNMENT (( #4572 ) ) ;
#9424 = CARTESIAN_POINT ( 'NONE',  ( -0.1306497350717320538, 6.000000000000001776, 4.000000000000004441 ) ) ;
#9425 = ORIENTED_EDGE ( 'NONE', *, *, #1450, .T. ) ;
#9426 = EDGE_CURVE ( 'NONE', #12333, #1040, #1868, .T. ) ;
#9427 = DIRECTION ( 'NONE',  ( 0.000000000000000000, 0.000000000000000000, -1.000000000000000000 ) ) ;
#9428 =( REPRESENTATION_RELATIONSHIP ('NONE','NONE', #11191, #4596 ) REPRESENTATION_RELATIONSHIP_WITH_TRANSFORMATION ( #7904 )SHAPE_REPRESENTATION_RELATIONSHIP( ) );
#9429 = CARTESIAN_POINT ( 'NONE',  ( 4.286401442266387640, 4.198423832313340043, 24.63239388001634111 ) ) ;
#9430 = DIRECTION ( 'NONE',  ( 0.000000000000000000, 0.000000000000000000, 1.000000000000000000 ) ) ;
#9431 = CARTESIAN_POINT ( 'NONE',  ( -4.070863287254169016, -4.743975846881727243, 18.87305891554299819 ) ) ;
#9432 = CARTESIAN_POINT ( 'NONE',  ( 4.592425496802573972E-16, -2.500000000000000000, 0.2999999999999999334 ) ) ;
#9433 = CARTESIAN_POINT ( 'NONE',  ( -4.344762547369802164, -4.493114738039127865, 25.00308643866044633 ) ) ;
#9434 =( NAMED_UNIT ( * ) PLANE_ANGLE_UNIT ( ) SI_UNIT ( $, .RADIAN. ) );
#9435 = CARTESIAN_POINT ( 'NONE',  ( 2.897581130414634077E-17, -9.750000000000003553, 0.000000000000000000 ) ) ;
#9436 = CARTESIAN_POINT ( 'NONE',  ( 1.767766952966369320, 184.7999999978150356, 5.232233047033630235 ) ) ;
#9437 = CARTESIAN_POINT ( 'NONE',  ( -0.06495987523897406302, 228.9118723585069120, 8.872930237925691799 ) ) ;
#9438 = CARTESIAN_POINT ( 'NONE',  ( 4.267936573529218514, 4.217499624512227818, 31.26229037835931379 ) ) ;
#9439 = EDGE_CURVE ( 'NONE', #4972, #4510, #3018, .T. ) ;
#9440 = EDGE_CURVE ( 'NONE', #14187, #11937, #6686, .T. ) ;
#9441 = CARTESIAN_POINT ( 'NONE',  ( -0.9975899816380627838, 189.4340297135221647, 4.147879558749815843 ) ) ;
#9442 = CARTESIAN_POINT ( 'NONE',  ( 2.500000000000000444, 187.2500000000000000, 5.964466094067262247 ) ) ;
#9443 = CARTESIAN_POINT ( 'NONE',  ( -2.500000000000000888, 188.3999999999999773, 7.000000000000000000 ) ) ;
#9445 = ORIENTED_EDGE ( 'NONE', *, *, #3406, .F. ) ;
#9444 = CYLINDRICAL_SURFACE ( 'NONE', #3439, 1.000000000000000000 ) ;
#9446 = CARTESIAN_POINT ( 'NONE',  ( -6.000000000000000000, 0.000000000000000000, 52.97056274847714263 ) ) ;
#9447 = DIRECTION ( 'NONE',  ( -0.000000000000000000, 1.000000000000000000, -0.000000000000000000 ) ) ;
#9448 =( REPRESENTATION_RELATIONSHIP ('NONE','NONE', #11191, #4596 ) REPRESENTATION_RELATIONSHIP_WITH_TRANSFORMATION ( #9814 )SHAPE_REPRESENTATION_RELATIONSHIP( ) );
#9449 = CARTESIAN_POINT ( 'NONE',  ( -5.385276659965230388E-16, 226.3251816629291966, 4.486670979098442480 ) ) ;
#9450 = CARTESIAN_POINT ( 'NONE',  ( -2.996310406655163572, 227.3383267913470149, 7.471278767517968156 ) ) ;
#9451 = CARTESIAN_POINT ( 'NONE',  ( 2.500000000000000000, 3.061616997868383141E-16, -0.1999999978150501789 ) ) ;
#9452 = CARTESIAN_POINT ( 'NONE',  ( -1.035533905932739529, 184.4800000002184959, 9.500000000000003553 ) ) ;
#9453 = LINE ( 'NONE', #1093, #5012 ) ;
#9454 = CARTESIAN_POINT ( 'NONE',  ( 1.132923824227977772, 228.7961917368426157, 8.538838004569329954 ) ) ;
#9455 = CARTESIAN_POINT ( 'NONE',  ( 5.570760634536790157, 2.834026536768273541, 11.23774718278288276 ) ) ;
#9456 = CARTESIAN_POINT ( 'NONE',  ( -0.8561741729129458411, -2.066987299999999195, 1.092474635061568626E-09 ) ) ;
#9457 = AXIS2_PLACEMENT_3D ( 'NONE', #9274, #13958, #6968 ) ;
#9458 = CARTESIAN_POINT ( 'NONE',  ( 1.500000000000000000, 9.750000000000003553, 2.000000000000001776 ) ) ;
#9459 = ORIENTED_EDGE ( 'NONE', *, *, #7284, .F. ) ;
#9460 = CARTESIAN_POINT ( 'NONE',  ( 0.8561741729129457301, 186.7999999989074809, 4.933012699999999029 ) ) ;
#9461 = ADVANCED_FACE ( 'NONE', ( #1814 ), #10105, .T. ) ;
#9462 = PRODUCT_DEFINITION_SHAPE ( 'NONE', 'NONE',  #15736 ) ;
#9463 = CARTESIAN_POINT ( 'NONE',  ( -1.000049560716488761, 5.916071405810155781, 11.36967799011531710 ) ) ;
#9464 = EDGE_LOOP ( 'NONE', ( #12270, #8192, #15549, #7255 ) ) ;
#9465 = CARTESIAN_POINT ( 'NONE',  ( -4.143041610105282935, -4.340967609747059086, 4.386022610569177971 ) ) ;
#9466 = CIRCLE ( 'NONE', #10986, 1.500000000000000000 ) ;
#9467 = CYLINDRICAL_SURFACE ( 'NONE', #11627, 1.000000000000000666 ) ;
#9468 = CARTESIAN_POINT ( 'NONE',  ( 5.665824935993625466, 1.978765057080873913, 17.00004946353775992 ) ) ;
#9469 = CARTESIAN_POINT ( 'NONE',  ( 2.066987300000000527, 185.8499999989074922, 7.000000000000000000 ) ) ;
#9470 = CARTESIAN_POINT ( 'NONE',  ( 2.782468714962263334, 5.316055268221493435, 18.50389795015982841 ) ) ;
#9471 = CARTESIAN_POINT ( 'NONE',  ( -2.500000000000000000, -1.035533905932739307, 1.050000002184949821 ) ) ;
#9472 = CARTESIAN_POINT ( 'NONE',  ( -5.903061651806607024, -2.057626436184781582, 4.000082581897114409 ) ) ;
#9473 = CARTESIAN_POINT ( 'NONE',  ( 0.000000000000000000, 186.5669965222008386, 9.317226423031119253 ) ) ;
#9474 = CARTESIAN_POINT ( 'NONE',  ( 0.000000000000000000, 0.000000000000000000, -13.50000000000000000 ) ) ;
#9475 = CARTESIAN_POINT ( 'NONE',  ( 13.50000000000000000, -0.001000000000000132727, -8.673617379884035472E-16 ) ) ;
#9476 =( BOUNDED_SURFACE ( )  B_SPLINE_SURFACE ( 1, 2, ( 
 ( #7083, #9386, #10426, #11919, #9235, #12798, #11763, #1900, #14224, #3179, #11690, #10502, #3331, #4454, #14149, #3251, #8118, #2056, #865, #8199, #10576, #13831, #8922, #12483, #2864, #7557, #390, #8691, #2944, #5178, #7792, #11215, #1505, #2785, #5260, #10107, #15037, #1739, #14962, #7638, #10184, #10262, #2707, #11368, #9954, #316, #3818, #6614, #1583, #4051, #10031, #13521, #13756, #240, #5416, #8763, #6381, #14879, #2628, #6461, #11293, #547, #12406, #11140, #5102, #7712, #12329, #12562, #1660, #6534, #7484, #470, #5341, #4131, #9003, #12639, #1424, #3968, #11446, #6299, #14805, #3890, #13597, #8842, #13674, #6688, #699, #2051, #6849, #936, #10339, #12789, #4526, #5573, #8193, #15353, #861, #4448, #6926, #7949, #13990 ),
 ( #10570, #7876, #11758, #7000, #9303, #4371, #14142, #9381, #3246, #8029, #8114, #3097, #11685, #4213, #14219, #10419, #3327, #6768, #1893, #14064, #784, #5647, #15427, #13028, #10497, #3172, #5728, #5802, #11600, #2127, #5495, #15270, #15115, #11829, #12867, #12951, #9230, #9083, #13908, #11522, #3020, #4291, #1971, #12717, #1816, #623, #15193, #9155, #9540, #13347, #1331, #9460, #3482, #7237, #9783, #14629, #3565, #12076, #11995, #8596, #13107, #9625, #15587, #2534, #10648, #4690, #4767, #14544, #13430, #8353, #11912, #2369, #1175, #9706, #6043, #1099, #2452, #1020, #5962, #8434, #15666, #8270, #5883, #10889, #1253, #7388, #10807, #12154, #14377, #3641, #5030, #7315, #3719, #13191, #4851, #3401, #8517, #6129, #10965, #7158, #2208 ) ),
 .UNSPECIFIED., .F., .F., .F. ) 
 B_SPLINE_SURFACE_WITH_KNOTS ( ( 2, 2 ),
 ( 3, 2, 2, 2, 2, 2, 2, 2, 2, 2, 2, 2, 2, 2, 2, 2, 2, 2, 2, 2, 2, 2, 2, 2, 2, 2, 2, 2, 2, 2, 2, 2, 2, 2, 2, 2, 2, 2, 2, 2, 2, 2, 2, 2, 2, 2, 2, 2, 2, 2, 3 ),
 ( 0.000000000000000000, 1.000000000000000000 ),
 ( 0.000000000000000000, 0.01785714285714285615, 0.03571428571428571230, 0.05357142857142856845, 0.07142857142857142461, 0.08928571428571428770, 0.1071428571428571369, 0.1250000000000000000, 0.1428571428571428492, 0.1607142857142857262, 0.1785714285714285754, 0.1964285714285714246, 0.2142857142857142738, 0.2321428571428571508, 0.2500000000000000000, 0.2678571428571428492, 0.2857142857142856984, 0.3035714285714285476, 0.3214285714285714524, 0.3392857142857143016, 0.3571428571428571508, 0.3750000000000000000, 0.3928571428571428492, 0.4107142857142856984, 0.4285714285714285476, 0.4464285714285714524, 0.4642857142857143016, 0.4821428571428571508, 0.5000000000000000000, 0.5178571428571429047, 0.5357142857142856984, 0.5535714285714286031, 0.5714285714285713969, 0.5892857142857143016, 0.6071428571428570953, 0.6250000000000000000, 0.6428571428571429047, 0.6607142857142856984, 0.6785714285714286031, 0.6964285714285713969, 0.7142857142857143016, 0.7321428571428570953, 0.7500000000000000000, 0.7678571428571429047, 0.7857142857142856984, 0.8035714285714286031, 0.8214285714285713969, 0.8392857142857143016, 0.8571428571428570953, 0.8750000000000000000, 0.8928571428571429047 ),
 .UNSPECIFIED. ) 
 GEOMETRIC_REPRESENTATION_ITEM ( )  RATIONAL_B_SPLINE_SURFACE ( (
 ( 1.000000000000000000, 0.9238795325112867385, 1.000000000000000000, 0.9238795325112867385, 1.000000000000000000, 0.9238795325112867385, 1.000000000000000000, 0.9238795325112867385, 1.000000000000000000, 0.9238795325112867385, 1.000000000000000000, 0.9238795325112867385, 1.000000000000000000, 0.9238795325112867385, 1.000000000000000000, 0.9238795325112867385, 1.000000000000000000, 0.9238795325112867385, 1.000000000000000000, 0.9238795325112867385, 1.000000000000000000, 0.9238795325112867385, 1.000000000000000000, 0.9238795325112867385, 1.000000000000000000, 0.9238795325112867385, 1.000000000000000000, 0.9238795325112867385, 1.000000000000000000, 0.9238795325112867385, 1.000000000000000000, 0.9238795325112867385, 1.000000000000000000, 0.9238795325112867385, 1.000000000000000000, 0.9238795325112867385, 1.000000000000000000, 0.9238795325112867385, 1.000000000000000000, 0.9238795325112867385, 1.000000000000000000, 0.9238795325112867385, 1.000000000000000000, 0.9238795325112867385, 1.000000000000000000, 0.9238795325112867385, 1.000000000000000000, 0.9238795325112867385, 1.000000000000000000, 0.9238795325112867385, 1.000000000000000000, 0.9238795325112867385, 1.000000000000000000, 0.9238795325112867385, 1.000000000000000000, 0.9238795325112867385, 1.000000000000000000, 0.9238795325112867385, 1.000000000000000000, 0.9238795325112867385, 1.000000000000000000, 0.9238795325112867385, 1.000000000000000000, 0.9238795325112867385, 1.000000000000000000, 0.9238795325112867385, 1.000000000000000000, 0.9238795325112867385, 1.000000000000000000, 0.9238795325112867385, 1.000000000000000000, 0.9238795325112867385, 1.000000000000000000, 0.9238795325112867385, 1.000000000000000000, 0.9238795325112867385, 1.000000000000000000, 0.9238795325112867385, 1.000000000000000000, 0.9238795325112867385, 1.000000000000000000, 0.9238795325112867385, 1.000000000000000000, 0.9238795325112867385, 1.000000000000000000, 0.9238795325112867385, 1.000000000000000000, 0.9238795325112867385, 1.000000000000000000, 0.9238795325112867385, 1.000000000000000000, 0.9238795325112867385, 1.000000000000000000, 0.9238795325112867385, 1.000000000000000000, 0.9238795325112867385, 1.000000000000000000, 0.9238795325112867385, 1.000000000000000000, 0.9238795325112867385, 1.000000000000000000),
 ( 1.000000000000000000, 0.9238795325112867385, 1.000000000000000000, 0.9238795325112867385, 1.000000000000000000, 0.9238795325112867385, 1.000000000000000000, 0.9238795325112867385, 1.000000000000000000, 0.9238795325112867385, 1.000000000000000000, 0.9238795325112867385, 1.000000000000000000, 0.9238795325112867385, 1.000000000000000000, 0.9238795325112867385, 1.000000000000000000, 0.9238795325112867385, 1.000000000000000000, 0.9238795325112867385, 1.000000000000000000, 0.9238795325112867385, 1.000000000000000000, 0.9238795325112867385, 1.000000000000000000, 0.9238795325112867385, 1.000000000000000000, 0.9238795325112867385, 1.000000000000000000, 0.9238795325112867385, 1.000000000000000000, 0.9238795325112867385, 1.000000000000000000, 0.9238795325112867385, 1.000000000000000000, 0.9238795325112867385, 1.000000000000000000, 0.9238795325112867385, 1.000000000000000000, 0.9238795325112867385, 1.000000000000000000, 0.9238795325112867385, 1.000000000000000000, 0.9238795325112867385, 1.000000000000000000, 0.9238795325112867385, 1.000000000000000000, 0.9238795325112867385, 1.000000000000000000, 0.9238795325112867385, 1.000000000000000000, 0.9238795325112867385, 1.000000000000000000, 0.9238795325112867385, 1.000000000000000000, 0.9238795325112867385, 1.000000000000000000, 0.9238795325112867385, 1.000000000000000000, 0.9238795325112867385, 1.000000000000000000, 0.9238795325112867385, 1.000000000000000000, 0.9238795325112867385, 1.000000000000000000, 0.9238795325112867385, 1.000000000000000000, 0.9238795325112867385, 1.000000000000000000, 0.9238795325112867385, 1.000000000000000000, 0.9238795325112867385, 1.000000000000000000, 0.9238795325112867385, 1.000000000000000000, 0.9238795325112867385, 1.000000000000000000, 0.9238795325112867385, 1.000000000000000000, 0.9238795325112867385, 1.000000000000000000, 0.9238795325112867385, 1.000000000000000000, 0.9238795325112867385, 1.000000000000000000, 0.9238795325112867385, 1.000000000000000000, 0.9238795325112867385, 1.000000000000000000, 0.9238795325112867385, 1.000000000000000000, 0.9238795325112867385, 1.000000000000000000, 0.9238795325112867385, 1.000000000000000000, 0.9238795325112867385, 1.000000000000000000, 0.9238795325112867385, 1.000000000000000000, 0.9238795325112867385, 1.000000000000000000) ) ) 
 REPRESENTATION_ITEM ( '' )  SURFACE ( )  );
#9477 = DIRECTION ( 'NONE',  ( 0.8090169943749506709, -0.5877852522924689183, 0.000000000000000000 ) ) ;
#9478 = ORIENTED_EDGE ( 'NONE', *, *, #11959, .F. ) ;
#9479 = ORIENTED_EDGE ( 'NONE', *, *, #2292, .T. ) ;
#9480 = VERTEX_POINT ( 'NONE', #14959 ) ;
#9481 = CARTESIAN_POINT ( 'NONE',  ( 4.435347140100995844, 4.403429997944549257, 31.00000000000000000 ) ) ;
#9482 = CARTESIAN_POINT ( 'NONE',  ( 7.490007020835728113, -2.433650805992114918, 17.99999999999998934 ) ) ;
#9483 = VERTEX_POINT ( 'NONE', #5414 ) ;
#9484 =( BOUNDED_CURVE ( )  B_SPLINE_CURVE ( 2, ( #8976, #1634, #11343, #7847, #13733, #11574, #2840, #10394, #599 ),
 .UNSPECIFIED., .F., .F. ) 
 B_SPLINE_CURVE_WITH_KNOTS ( ( 3, 2, 2, 2, 3 ),
 ( 0.7857142857142856984, 0.8035714285714286031, 0.8214285714285713969, 0.8392857142857143016, 0.8571428571428570953 ),
 .UNSPECIFIED. ) 
 CURVE ( )  GEOMETRIC_REPRESENTATION_ITEM ( )  RATIONAL_B_SPLINE_CURVE ( ( 1.000000000000000000, 0.9238795325112867385, 1.000000000000000000, 0.9238795325112867385, 1.000000000000000000, 0.9238795325112867385, 1.000000000000000000, 0.9238795325112867385, 1.000000000000000000 ) ) 
 REPRESENTATION_ITEM ( '' )  );
#9485 = EDGE_CURVE ( 'NONE', #14187, #4873, #14574, .T. ) ;
#9486 = CARTESIAN_POINT ( 'NONE',  ( -1.530808498934191571E-16, 2.500000000000000000, -3.199999997815050623 ) ) ;
#9487 = CARTESIAN_POINT ( 'NONE',  ( 0.1323933160975658274, -6.000000000000000000, 6.000000000000003553 ) ) ;
#9488 = CARTESIAN_POINT ( 'NONE',  ( -2.817313151351109379, -5.579000502529473771, 4.867625892836954904 ) ) ;
#9489 = CARTESIAN_POINT ( 'NONE',  ( 0.8561741729129455081, 186.1999999989075150, 4.933012699999999029 ) ) ;
#9490 = CARTESIAN_POINT ( 'NONE',  ( -1.767766952966369098, 1.767766952966369098, -1.593000000021849827 ) ) ;
#9491 = LINE ( 'NONE', #970, #2868 ) ;
#9492 = APPLICATION_PROTOCOL_DEFINITION ( 'draft international standard', 'automotive_design', 1998, #12070 ) ;
#9493 = CARTESIAN_POINT ( 'NONE',  ( 2.066987299999999639, 2.531329380823229670E-16, 0.8500000010924746441 ) ) ;
#9494 = DIRECTION ( 'NONE',  ( 0.000000000000000000, 0.000000000000000000, 1.000000000000000000 ) ) ;
#9495 = CARTESIAN_POINT ( 'NONE',  ( 2.990158053860457077, 227.3692281962998436, 7.562228658338257858 ) ) ;
#9496 = CARTESIAN_POINT ( 'NONE',  ( 0.000000000000000000, 184.0000000000000000, 7.000000000000000000 ) ) ;
#9497 = EDGE_LOOP ( 'NONE', ( #5966, #9624 ) ) ;
#9498 = VERTEX_POINT ( 'NONE', #6379 ) ;
#9499 = CARTESIAN_POINT ( 'NONE',  ( 6.000000000000000888, 7.347880794884120722E-16, 53.67766952966368876 ) ) ;
#9500 = ORIENTED_EDGE ( 'NONE', *, *, #4773, .F. ) ;
#9501 = VERTEX_POINT ( 'NONE', #13829 ) ;
#9502 = CARTESIAN_POINT ( 'NONE',  ( 0.5030929395820508132, 6.230885867001143552, 30.12600319116549485 ) ) ;
#9503 = EDGE_CURVE ( 'NONE', #7387, #2947, #940, .T. ) ;
#9504 = CARTESIAN_POINT ( 'NONE',  ( 2.668367453516584220, -5.373994336898154422, 17.99999999999998934 ) ) ;
#9505 = CARTESIAN_POINT ( 'NONE',  ( -4.196288036172508562, -4.288789315524776491, 25.00312048902377882 ) ) ;
#9506 = ORIENTED_EDGE ( 'NONE', *, *, #10911, .F. ) ;
#9507 = ADVANCED_FACE ( 'NONE', ( #12715 ), #5176, .F. ) ;
#9508 = CARTESIAN_POINT ( 'NONE',  ( -6.081509788407757355, 1.446521464462645401, 31.87381964045071214 ) ) ;
#9509 = CARTESIAN_POINT ( 'NONE',  ( 4.286401442266388528, 4.198423832313340043, 24.49999999999999289 ) ) ;
#9510 = LINE ( 'NONE', #6969, #12995 ) ;
#9511 = CARTESIAN_POINT ( 'NONE',  ( -2.931156713028535865, 5.520271803279187317, 12.00436969680153076 ) ) ;
#9512 = CARTESIAN_POINT ( 'NONE',  ( -2.500000000000000000, -1.035533905932739307, -2.250000000000000444 ) ) ;
#9513 = CARTESIAN_POINT ( 'NONE',  ( -2.997753866155913549, -5.484939622623791422, 25.11560192892921606 ) ) ;
#9514 = EDGE_CURVE ( 'NONE', #13977, #2787, #13906, .T. ) ;
#9515 = DIRECTION ( 'NONE',  ( 1.000000000000000000, 0.000000000000000000, 0.000000000000000000 ) ) ;
#9516 = CARTESIAN_POINT ( 'NONE',  ( 1.767766952966369098, 189.5999999978150470, 5.232233047033630235 ) ) ;
#9517 = CARTESIAN_POINT ( 'NONE',  ( -1.886200273035058439, 228.4697824026276294, 7.596149230188033563 ) ) ;
#9518 = CARTESIAN_POINT ( 'NONE',  ( 4.005998022989950336, 4.467726698309270716, 31.79931806258174021 ) ) ;
#9519 = CARTESIAN_POINT ( 'NONE',  ( -0.3320323468824299962, 190.0863194065883022, 4.213467285827682041 ) ) ;
#9520 = ORIENTED_EDGE ( 'NONE', *, *, #8312, .T. ) ;
#9521 = CARTESIAN_POINT ( 'NONE',  ( -3.107583187530425839, 5.133966411712686195, 4.126193172852896218 ) ) ;
#9522 = CYLINDRICAL_SURFACE ( 'NONE', #14272, 1.000000000000000666 ) ;
#9524 = ORIENTED_EDGE ( 'NONE', *, *, #14388, .T. ) ;
#9523 = DIRECTION ( 'NONE',  ( -0.9510565162951544194, 0.3090169943749447312, 0.000000000000000000 ) ) ;
#9525 = CYLINDRICAL_SURFACE ( 'NONE', #13134, 1.999999999999999556 ) ;
#9526 = DIRECTION ( 'NONE',  ( -0.9510565162951545304, 0.3090169943749447867, 0.000000000000000000 ) ) ;
#9527 = ORIENTED_EDGE ( 'NONE', *, *, #1853, .F. ) ;
#9528 = CARTESIAN_POINT ( 'NONE',  ( -5.903057025253903412, -1.078199533779516495, 30.38438267301394191 ) ) ;
#9529 = VECTOR ( 'NONE', #15365, 1000.000000000000114 ) ;
#9530 = CARTESIAN_POINT ( 'NONE',  ( 1.461580736456472573, 1.461580736456472795, 1.950000001092474955 ) ) ;
#9531 = CARTESIAN_POINT ( 'NONE',  ( -2.817344785281778563, 226.9578842961288103, 6.351048551979458168 ) ) ;
#9532 = CARTESIAN_POINT ( 'NONE',  ( 6.155973317223311092, 1.081218830693581268, 25.00308643866044989 ) ) ;
#9533 = CARTESIAN_POINT ( 'NONE',  ( 1.035533905932738197, 186.1800000002184845, 9.500000000000003553 ) ) ;
#9534 = DIRECTION ( 'NONE',  ( 0.5877852522924802425, -0.8090169943749422332, 0.000000000000000000 ) ) ;
#9535 = CARTESIAN_POINT ( 'NONE',  ( -0.3251550031287174236, 227.6173728764936186, 5.134341900458684549 ) ) ;
#9536 = CARTESIAN_POINT ( 'NONE',  ( 5.616089948629710449, 2.743103014345580348, 10.99563030319847279 ) ) ;
#9537 = CARTESIAN_POINT ( 'NONE',  ( 2.066987299999999639, 2.531329380823229670E-16, 1.850000001092474866 ) ) ;
#9538 = CARTESIAN_POINT ( 'NONE',  ( 5.725930890718329280, 2.506952462184043995, 17.20066851092422411 ) ) ;
#9539 = ORIENTED_EDGE ( 'NONE', *, *, #8766, .T. ) ;
#9540 = CARTESIAN_POINT ( 'NONE',  ( 2.066987300000000527, 186.6499999989075320, 7.000000000000000000 ) ) ;
#9541 = CARTESIAN_POINT ( 'NONE',  ( -5.285485590866834116E-16, 186.4499999989075150, 9.066987300000000971 ) ) ;
#9542 = CARTESIAN_POINT ( 'NONE',  ( 5.843075991566612615, 1.368655265450926528, 23.62635295315577011 ) ) ;
#9543 = VECTOR ( 'NONE', #7046, 1000.000000000000000 ) ;
#9544 = ORIENTED_EDGE ( 'NONE', *, *, #582, .T. ) ;
#9545 = CARTESIAN_POINT ( 'NONE',  ( -2.849269941561920927, -5.281123252784068356, 4.384806175511482884 ) ) ;
#9546 = B_SPLINE_CURVE_WITH_KNOTS ( 'NONE', 3,
 ( #12606, #1704, #6580, #10000, #13638, #8731, #2673, #11415, #516, #7525, #12371, #1469, #7604, #12452, #1552, #5228, #12990, #8076 ),
 .UNSPECIFIED., .F., .F.,
 ( 4, 2, 2, 2, 2, 2, 2, 2, 4 ),
 ( 0.000000000000000000, 0.0003914357524127466724, 0.0007828715048254933449, 0.001174307257238240126, 0.001565743009650986690, 0.001957178762063733254, 0.002348614514476480251, 0.002740050266889226815, 0.003131486019301973379 ),
 .UNSPECIFIED. ) ;
#9547 = CARTESIAN_POINT ( 'NONE',  ( 5.409274167810653289, -2.597759609440645878, 5.615193824488510010 ) ) ;
#9548 = ADVANCED_FACE ( 'NONE', ( #1581 ), #3966, .F. ) ;
#9549 = DIRECTION ( 'NONE',  ( 0.000000000000000000, 0.000000000000000000, 1.000000000000000000 ) ) ;
#9550 = DIRECTION ( 'NONE',  ( 0.5877852522924802425, -0.8090169943749422332, 0.000000000000000000 ) ) ;
#9551 = CARTESIAN_POINT ( 'NONE',  ( 0.8561741729129457301, 185.9999999989074979, 4.933012699999999029 ) ) ;
#9552 = CARTESIAN_POINT ( 'NONE',  ( 2.668367453516506949, 5.373994336898193502, 18.13064961348854709 ) ) ;
#9553 = CARTESIAN_POINT ( 'NONE',  ( 2.500000000000000000, 3.061616997868383141E-16, 0.6000000021849497545 ) ) ;
#9554 = CARTESIAN_POINT ( 'NONE',  ( 4.286401442266544848, -4.198423832313181059, 11.49999999999998224 ) ) ;
#9555 = CARTESIAN_POINT ( 'NONE',  ( 0.8499999999999896527, 0.4000000000000062395, 2.749999999999994227 ) ) ;
#9556 = CARTESIAN_POINT ( 'NONE',  ( 1.000049271338508516, -6.169473353325548359, 30.86969612704550414 ) ) ;
#9557 = CARTESIAN_POINT ( 'NONE',  ( -5.726307184802641004, 2.506131700382491445, 10.69973484982323519 ) ) ;
#9558 = CARTESIAN_POINT ( 'NONE',  ( 1.354942164306246880E-13, -6.000000000000000888, 16.99999999999998579 ) ) ;
#9559 = ORIENTED_EDGE ( 'NONE', *, *, #12454, .T. ) ;
#9560 = EDGE_LOOP ( 'NONE', ( #1745, #9252, #11828, #14417, #4870, #4810 ) ) ;
#9561 = ORIENTED_EDGE ( 'NONE', *, *, #2836, .T. ) ;
#9562 = CARTESIAN_POINT ( 'NONE',  ( 6.176542424588106428, 0.9554180641286317277, 4.869360672457872852 ) ) ;
#9563 = ORIENTED_EDGE ( 'NONE', *, *, #1067, .T. ) ;
#9564 = CARTESIAN_POINT ( 'NONE',  ( -2.500000000000000444, 1.035533905932737753, -3.049999997815050268 ) ) ;
#9565 = CARTESIAN_POINT ( 'NONE',  ( -5.903119516422473012, -1.077859910107510588, 31.61519382448851090 ) ) ;
#9566 = CARTESIAN_POINT ( 'NONE',  ( -2.500000000000000444, 1.035533905932737753, 0.05000000000000013461 ) ) ;
#9567 = CARTESIAN_POINT ( 'NONE',  ( 0.8561741729129455081, 186.9999999989074979, 4.933012699999999029 ) ) ;
#9568 = CARTESIAN_POINT ( 'NONE',  ( 2.500000000000000444, -1.035533905932737309, -0.3430000000218496048 ) ) ;
#9569 = SHAPE_REPRESENTATION ( 'strain limiting mesh layer', ( #14201 ), #10667 ) ;
#9570 = CARTESIAN_POINT ( 'NONE',  ( -5.558508435838166228, 2.857531096718976649, 17.99999999999998934 ) ) ;
#9571 = CARTESIAN_POINT ( 'NONE',  ( -1.461580736456472795, 1.461580736456472795, -2.849999998907525089 ) ) ;
#9572 = CARTESIAN_POINT ( 'NONE',  ( 3.159612573729317919, -5.393342049074581368, 4.199734849823245852 ) ) ;
#9573 = CARTESIAN_POINT ( 'NONE',  ( -0.6817270424356797198, 226.3498696214933545, 4.559454910794151772 ) ) ;
#9574 = VECTOR ( 'NONE', #5078, 1000.000000000000000 ) ;
#9575 = CYLINDRICAL_SURFACE ( 'NONE', #14338, 2.500000000000000444 ) ;
#9576 = VERTEX_POINT ( 'NONE', #6924 ) ;
#9577 = VERTEX_POINT ( 'NONE', #5881 ) ;
#9578 = FACE_OUTER_BOUND ( 'NONE', #3272, .T. ) ;
#9579 = ORIENTED_EDGE ( 'NONE', *, *, #10572, .F. ) ;
#9580 = ORIENTED_EDGE ( 'NONE', *, *, #8261, .F. ) ;
#9581 = CARTESIAN_POINT ( 'NONE',  ( 0.7995524673975824559, 6.199337389817267230, 31.61453679452459653 ) ) ;
#9582 = CARTESIAN_POINT ( 'NONE',  ( -4.435347140101154828, -4.403429997944389385, 24.49999999999999289 ) ) ;
#9583 = B_SPLINE_CURVE_WITH_KNOTS ( 'NONE', 3,
 ( #3093, #620, #11597, #858, #3168, #11519, #15190, #12864, #9227, #4367, #2124, #9152, #12786, #11826, #5725, #4288, #2048, #13905 ),
 .UNSPECIFIED., .F., .F.,
 ( 4, 2, 2, 2, 2, 2, 2, 2, 4 ),
 ( 0.000000000000000000, 0.0003914357524127480819, 0.0007828715048254961638, 0.001174307257238244246, 0.001565743009650992328, 0.001957178762063741060, 0.002348614514476489792, 0.002740050266889238525, 0.003131486019301987257 ),
 .UNSPECIFIED. ) ;
#9584 = CARTESIAN_POINT ( 'NONE',  ( -3.107583187530525315, -5.133966411712624023, 25.37380682714709579 ) ) ;
#9585 = CARTESIAN_POINT ( 'NONE',  ( 4.435347140101025154, -4.403429997944519059, 11.49999999999998224 ) ) ;
#9586 = CARTESIAN_POINT ( 'NONE',  ( 4.195842658231335065, 4.289229542213299773, 25.00439760644211518 ) ) ;
#9587 = CARTESIAN_POINT ( 'NONE',  ( 4.000000000000002665, 184.0000000000000000, -7.000000000000000888 ) ) ;
#9588 = CARTESIAN_POINT ( 'NONE',  ( -3.567624405365362072, 5.133384272590696185, 12.49995078984291830 ) ) ;
#9589 = CARTESIAN_POINT ( 'NONE',  ( 5.329945432499583191, 2.755769831645226375, 30.73770962164068266 ) ) ;
#9590 = DIRECTION ( 'NONE',  ( 0.8090169943749506709, -0.5877852522924686962, 0.000000000000000000 ) ) ;
#9591 = CARTESIAN_POINT ( 'NONE',  ( 6.805491029613696752E-14, 146.0000000000000000, -9.750000000000003553 ) ) ;
#9592 = PRODUCT_DEFINITION_SHAPE ( 'NONE', 'NONE',  #15760 ) ;
#9593 = CARTESIAN_POINT ( 'NONE',  ( -2.500000000000000888, 188.3499999978150186, 8.035533905932737753 ) ) ;
#9594 = EDGE_CURVE ( 'NONE', #5121, #12426, #9228, .T. ) ;
#9595 = CARTESIAN_POINT ( 'NONE',  ( 2.191560967657306680, 226.6301005958437145, 5.385416860794732585 ) ) ;
#9596 = PRODUCT_DEFINITION_FORMATION_WITH_SPECIFIED_SOURCE ( 'ANY', '', #2311, .NOT_KNOWN. ) ;
#9597 = CARTESIAN_POINT ( 'NONE',  ( 5.616116467183692507, -2.743044348085474038, 17.49574050496990907 ) ) ;
#9598 = ADVANCED_FACE ( 'NONE', ( #11756 ), #15508, .F. ) ;
#9599 = AXIS2_PLACEMENT_3D ( 'NONE', #6411, #14512, #11088 ) ;
#9600 = FACE_OUTER_BOUND ( 'NONE', #11799, .T. ) ;
#9601 = B_SPLINE_CURVE_WITH_KNOTS ( 'NONE', 3,
 ( #11477, #505, #7825, #8882, #7747, #6416, #4324, #13714, #2822, #6568, #12593, #581, #7903, #7670, #5450, #10296, #5374, #12518 ),
 .UNSPECIFIED., .F., .F.,
 ( 4, 2, 2, 2, 2, 2, 2, 2, 4 ),
 ( 0.003131918686235976926, 0.003523310662250266762, 0.003914702638264556597, 0.004306094614278846433, 0.004697486590293136269, 0.005088878566307426105, 0.005480270542321715940, 0.005871662518336004041, 0.006263054494350293010 ),
 .UNSPECIFIED. ) ;
#9602 = EDGE_LOOP ( 'NONE', ( #7257, #8889, #13130, #6083 ) ) ;
#9603 = LINE ( 'NONE', #15570, #3510 ) ;
#9604 = CARTESIAN_POINT ( 'NONE',  ( 1.000049560716623098, -5.916071405810133577, 11.36967799011532598 ) ) ;
#9605 = B_SPLINE_CURVE_WITH_KNOTS ( 'NONE', 3,
 ( #12604, #1389, #2671, #15008, #434, #1550, #11102, #10229, #15081, #8656, #204, #5308, #9918, #12528, #7523, #12369, #4098, #13798 ),
 .UNSPECIFIED., .F., .F.,
 ( 4, 2, 2, 2, 2, 2, 2, 2, 4 ),
 ( 0.000000000000000000, 0.0003914357524127471603, 0.0007828715048254943206, 0.001174307257238241644, 0.001565743009650988641, 0.001957178762063735422, 0.002348614514476481552, 0.002740050266889228116, 0.003131486019301974680 ),
 .UNSPECIFIED. ) ;
#9607 = VERTEX_POINT ( 'NONE', #1018 ) ;
#9606 = CARTESIAN_POINT ( 'NONE',  ( 2.668367453516610865, 5.373994336898140212, 31.00000000000000000 ) ) ;
#9608 = DIRECTION ( 'NONE',  ( 0.8660254037844400399, 0.000000000000000000, 0.4999999999999975020 ) ) ;
#9609 = DIRECTION ( 'NONE',  ( -6.123233995736766036E-17, 1.000000000000000000, 0.000000000000000000 ) ) ;
#9610 = AXIS2_PLACEMENT_3D ( 'NONE', #10110, #11372, #3173 ) ;
#9611 = DIRECTION ( 'NONE',  ( -1.000000000000000000, 3.326610055774637112E-18, 1.062480551894331163E-17 ) ) ;
#9612 = VECTOR ( 'NONE', #11840, 1000.000000000000000 ) ;
#9613 = CARTESIAN_POINT ( 'NONE',  ( -0.8561741729129455081, 2.066987299999999639, 1.300000001092474822 ) ) ;
#9614 = CARTESIAN_POINT ( 'NONE',  ( -1.191764142581503760, 226.4044614763379855, 4.720388933816794363 ) ) ;
#9615 = CARTESIAN_POINT ( 'NONE',  ( -0.8738239080080079102, -6.188820299975598793, 31.50355795710144946 ) ) ;
#9616 = CARTESIAN_POINT ( 'NONE',  ( -2.500000000000000888, 188.3300000002184902, 7.000000000000000000 ) ) ;
#9617 = CARTESIAN_POINT ( 'NONE',  ( -3.882673863916280332, 4.899192824800945978, 5.974085423341712442 ) ) ;
#9618 = CARTESIAN_POINT ( 'NONE',  ( 0.8230742150784297051, 227.6668866512619047, 5.277340506070477666 ) ) ;
#9619 = B_SPLINE_CURVE_WITH_KNOTS ( 'NONE', 3,
 ( #5636, #9291, #3233, #8100, #6911, #4511, #11746, #5713, #4595, #10557, #14207, #8177, #13015, #2115, #921, #15499, #3387, #14360 ),
 .UNSPECIFIED., .F., .F.,
 ( 4, 2, 2, 2, 2, 2, 2, 2, 4 ),
 ( 0.003131486019301970777, 0.003522824630466679218, 0.003914163241631387659, 0.004305501852796096533, 0.004696840463960804540, 0.005088179075125513415, 0.005479517686290222289, 0.005870856297454931164, 0.006262194908619639171 ),
 .UNSPECIFIED. ) ;
#9620 = EDGE_CURVE ( 'NONE', #12135, #6615, #12039, .T. ) ;
#9621 = CARTESIAN_POINT ( 'NONE',  ( 1.496490727326450720, 228.6905582067893477, 8.233762344832721070 ) ) ;
#9622 = CARTESIAN_POINT ( 'NONE',  ( 3.796994071234844259E-16, -2.066987299999999639, 0.05000000109247476621 ) ) ;
#9623 = CARTESIAN_POINT ( 'NONE',  ( 0.000000000000000000, 184.0000000000000000, 7.000000000000000000 ) ) ;
#9624 = ORIENTED_EDGE ( 'NONE', *, *, #5981, .F. ) ;
#9625 = CARTESIAN_POINT ( 'NONE',  ( 0.8561741729129460632, 187.2999999989075661, 9.066987300000000971 ) ) ;
#9626 = VECTOR ( 'NONE', #1861, 1000.000000000000000 ) ;
#9627 = CARTESIAN_POINT ( 'NONE',  ( -2.066987300000000527, 184.6499999989075320, 7.000000000000000000 ) ) ;
#9628 = CARTESIAN_POINT ( 'NONE',  ( -2.500000000000000444, 187.4999999978150527, 7.000000000000000000 ) ) ;
#9629 = VERTEX_POINT ( 'NONE', #8268 ) ;
#9630 =( NAMED_UNIT ( * ) PLANE_ANGLE_UNIT ( ) SI_UNIT ( $, .RADIAN. ) );
#9631 = FACE_OUTER_BOUND ( 'NONE', #15532, .T. ) ;
#9632 = CARTESIAN_POINT ( 'NONE',  ( 5.999999999999999112, 221.4150671951173592, 6.196499129422101682 ) ) ;
#9633 = CARTESIAN_POINT ( 'NONE',  ( 2.066987300000000083, 188.2499999989075263, 7.000000000000000000 ) ) ;
#9634 = VECTOR ( 'NONE', #15631, 1000.000000000000000 ) ;
#9635 = DIRECTION ( 'NONE',  ( -0.8660254037844387076, -0.4999999999999998890, 0.000000000000000000 ) ) ;
#9636 = CARTESIAN_POINT ( 'NONE',  ( -3.000000000000000000, 1.732050807568877415, -5.500000000000000000 ) ) ;
#9637 = DIRECTION ( 'NONE',  ( 0.000000000000000000, 0.000000000000000000, 1.000000000000000000 ) ) ;
#9638 = CARTESIAN_POINT ( 'NONE',  ( 5.409274167810663947, -2.597759609440622341, 31.61519382448851090 ) ) ;
#9639 = CARTESIAN_POINT ( 'NONE',  ( 2.500000000000000444, 1.035533905932737975, 0.5499999999999999334 ) ) ;
#9640 = CARTESIAN_POINT ( 'NONE',  ( -5.984595133899179409, 1.806709459528658135, 10.50004921015705150 ) ) ;
#9641 = CARTESIAN_POINT ( 'NONE',  ( -1.035533905932737975, 187.4500000000000171, 4.500000000000001776 ) ) ;
#9642 = ORIENTED_EDGE ( 'NONE', *, *, #12036, .F. ) ;
#9643 = EDGE_CURVE ( 'NONE', #7578, #9215, #2470, .T. ) ;
#9644 = VERTEX_POINT ( 'NONE', #4606 ) ;
#9645 = APPLICATION_CONTEXT ( 'automotive_design' ) ;
#9646 = ORIENTED_EDGE ( 'NONE', *, *, #8965, .F. ) ;
#9647 = CARTESIAN_POINT ( 'NONE',  ( -2.849269941562057262, 5.281123252783995525, 12.11519382448850557 ) ) ;
#9648 = EDGE_CURVE ( 'NONE', #10893, #878, #859, .T. ) ;
#9649 = ORIENTED_EDGE ( 'NONE', *, *, #2892, .F. ) ;
#9650 = CARTESIAN_POINT ( 'NONE',  ( -2.066987299999999639, 0.000000000000000000, 2.050000001092474822 ) ) ;
#9651 = DIRECTION ( 'NONE',  ( 1.000000000000000000, 0.000000000000000000, 0.000000000000000000 ) ) ;
#9652 = CARTESIAN_POINT ( 'NONE',  ( 6.176542424588109093, 0.9554180641286111886, 31.00000000000000000 ) ) ;
#9653 = CARTESIAN_POINT ( 'NONE',  ( -0.8561741729129456191, 188.6999999989075150, 4.933012699999999029 ) ) ;
#9654 = CARTESIAN_POINT ( 'NONE',  ( -1.767766952966368432, -1.767766952966369320, 1.006999999978150484 ) ) ;
#9655 = CARTESIAN_POINT ( 'NONE',  ( -2.668367453516691690, -5.373994336898102020, 11.49999999999998224 ) ) ;
#9656 = CONTEXT_DEPENDENT_SHAPE_REPRESENTATION ( #14934, #63 ) ;
#9657 = PRESENTATION_LAYER_ASSIGNMENT (  '', '', ( #4319 ) ) ;
#9658 = CARTESIAN_POINT ( 'NONE',  ( 2.066987299999999639, 2.531329380823229670E-16, -2.349999998907525534 ) ) ;
#9659 = LINE ( 'NONE', #15619, #7583 ) ;
#9660 = CARTESIAN_POINT ( 'NONE',  ( -1.328763708711319325, 228.1557872355912195, 9.876186263205003257 ) ) ;
#9661 = DIRECTION ( 'NONE',  ( -6.123233995736766036E-17, 1.000000000000000000, 0.000000000000000000 ) ) ;
#9662 = ORIENTED_EDGE ( 'NONE', *, *, #7211, .T. ) ;
#9663 = ORIENTED_EDGE ( 'NONE', *, *, #524, .T. ) ;
#9664 = CARTESIAN_POINT ( 'NONE',  ( 4.435347140100961205, 4.403429997944583008, 11.49999999999998224 ) ) ;
#9665 = ORIENTED_EDGE ( 'NONE', *, *, #2036, .T. ) ;
#9666 = EDGE_LOOP ( 'NONE', ( #9727, #5366, #15237, #13699 ) ) ;
#9667 = CARTESIAN_POINT ( 'NONE',  ( -5.725684683139557585, 2.507514573674882286, 25.29887838423338309 ) ) ;
#9668 = CARTESIAN_POINT ( 'NONE',  ( 0.000000000000000000, 0.000000000000000000, 0.000000000000000000 ) ) ;
#9669 = AXIS2_PLACEMENT_3D ( 'NONE', #11655, #10545, #9679 ) ;
#9670 = CARTESIAN_POINT ( 'NONE',  ( 0.1323736289504360564, -6.250000000000000000, 6.000000000000007105 ) ) ;
#9671 =( BOUNDED_CURVE ( )  B_SPLINE_CURVE ( 2, ( #13035, #5889, #3407, #12874, #8038, #15278, #9309, #10655, #15435 ),
 .UNSPECIFIED., .F., .F. ) 
 B_SPLINE_CURVE_WITH_KNOTS ( ( 3, 2, 2, 2, 3 ),
 ( 0.2857142857142856984, 0.3035714285714285476, 0.3214285714285714524, 0.3392857142857143016, 0.3571428571428571508 ),
 .UNSPECIFIED. ) 
 CURVE ( )  GEOMETRIC_REPRESENTATION_ITEM ( )  RATIONAL_B_SPLINE_CURVE ( ( 1.000000000000000000, 0.9238795325112867385, 1.000000000000000000, 0.9238795325112867385, 1.000000000000000000, 0.9238795325112867385, 1.000000000000000000, 0.9238795325112867385, 1.000000000000000000 ) ) 
 REPRESENTATION_ITEM ( '' )  );
#9672 = CARTESIAN_POINT ( 'NONE',  ( -5.558508435838220407, 2.857531096718872732, 31.13060690723498780 ) ) ;
#9673 = UNCERTAINTY_MEASURE_WITH_UNIT (LENGTH_MEASURE( 1.000000000000000082E-05 ), #2841, 'distance_accuracy_value', 'NONE');
#9674 = CYLINDRICAL_SURFACE ( 'NONE', #9599, 1.000000000000000666 ) ;
#9675 = DIRECTION ( 'NONE',  ( 0.000000000000000000, 0.000000000000000000, -1.000000000000000000 ) ) ;
#9676 = CARTESIAN_POINT ( 'NONE',  ( 2.500000000000000000, 3.061616997868383141E-16, -0.9999999978150501123 ) ) ;
#9677 = CARTESIAN_POINT ( 'NONE',  ( 5.915699123067156506, 1.003533581835566846, 30.49610204984016448 ) ) ;
#9678 = CARTESIAN_POINT ( 'NONE',  ( 0.8002302970948492744, -5.947135855825840700, 23.88601773212297630 ) ) ;
#9679 = DIRECTION ( 'NONE',  ( 1.000000000000000000, 0.000000000000000000, 0.000000000000000000 ) ) ;
#9680 = CARTESIAN_POINT ( 'NONE',  ( -1.767766952966369320, 188.1999999978150697, 5.232233047033630235 ) ) ;
#9681 = CARTESIAN_POINT ( 'NONE',  ( 1.240393925004889208, 226.4108590421392933, 4.739248726333301853 ) ) ;
#9682 = CARTESIAN_POINT ( 'NONE',  ( 3.421280866381124497, 4.930711975950923254, 32.00004932073312602 ) ) ;
#9683 = CARTESIAN_POINT ( 'NONE',  ( 5.487097279078418488, 2.429065649168846708, 31.79952054102715309 ) ) ;
#9684 = ORIENTED_EDGE ( 'NONE', *, *, #11916, .F. ) ;
#9685 = DIRECTION ( 'NONE',  ( 1.000000000000000000, 0.000000000000000000, 0.000000000000000000 ) ) ;
#9686 = CARTESIAN_POINT ( 'NONE',  ( -1.000079958708067318, -5.916066267613712348, 11.63152738882033965 ) ) ;
#9688 = ORIENTED_EDGE ( 'NONE', *, *, #2036, .F. ) ;
#9687 = CARTESIAN_POINT ( 'NONE',  ( -4.286401442266737583, 4.198423832312984771, 24.49999999999999289 ) ) ;
#9689 = CARTESIAN_POINT ( 'NONE',  ( 0.02317000962515113754, -0.3999999999999923617, 2.516813694799619139 ) ) ;
#9690 = CARTESIAN_POINT ( 'NONE',  ( 2.500000000000000444, 184.0000000000000000, 7.000000000000000000 ) ) ;
#9691 = ORIENTED_EDGE ( 'NONE', *, *, #11482, .F. ) ;
#9692 = CARTESIAN_POINT ( 'NONE',  ( 2.000000000000001776, 0.000000000000000000, 0.000000000000000000 ) ) ;
#9693 = EDGE_CURVE ( 'NONE', #6042, #3644, #2890, .T. ) ;
#9694 = B_SPLINE_CURVE_WITH_KNOTS ( 'NONE', 3,
 ( #13826, #6376, #11363, #13751, #10258, #12323, #8998, #10025, #7633, #5173, #1500, #13667, #8837, #3885, #14800, #15110, #2780, #311, #2859, #2939, #1732, #9948, #12633, #3963, #7787, #542, #1578, #6456, #2701, #11288, #3014, #4208 ),
 .UNSPECIFIED., .F., .F.,
 ( 4, 2, 2, 2, 2, 2, 2, 2, 2, 2, 2, 2, 2, 2, 2, 4 ),
 ( 0.000000000000000000, 0.0005931748005980339630, 0.001186349601196067926, 0.001779524401794101889, 0.002372699202392135852, 0.002965874002990170465, 0.003559048803588205946, 0.004152223604186240126, 0.004745398404784276040, 0.005338573205382311088, 0.005931748005980345267, 0.007118097607176415362, 0.007711272407774453011, 0.008304447208372488926, 0.008897622008970526575, 0.009490796809568564224 ),
 .UNSPECIFIED. ) ;
#9695 = CARTESIAN_POINT ( 'NONE',  ( 2.066987300000000083, -0.8561741729129449530, 1.000000001092474777 ) ) ;
#9696 = CARTESIAN_POINT ( 'NONE',  ( 5.783198643800774086, -1.602922020054686758, 4.026221760567070262 ) ) ;
#9697 =( NAMED_UNIT ( * ) PLANE_ANGLE_UNIT ( ) SI_UNIT ( $, .RADIAN. ) );
#9698 = CARTESIAN_POINT ( 'NONE',  ( -5.903061651806607912, 2.057626436184776697, 12.49991741810287138 ) ) ;
#9699 = CARTESIAN_POINT ( 'NONE',  ( -1.767766952966369765, 188.4300000002185129, 8.767766952966368876 ) ) ;
#9700 = CARTESIAN_POINT ( 'NONE',  ( -1.889311774764879104, 228.4700178340609114, 7.596829169595165077 ) ) ;
#9701 = CARTESIAN_POINT ( 'NONE',  ( 0.9660064634511277282, 228.8301302322938966, 8.636854315157751927 ) ) ;
#9702 = CARTESIAN_POINT ( 'NONE',  ( -1.461580736456472351, -1.461580736456473018, 0.7500000010924748883 ) ) ;
#9703 = CARTESIAN_POINT ( 'NONE',  ( 5.570760634536824796, 2.834026536768204263, 17.73774718278285434 ) ) ;
#9704 = ORIENTED_EDGE ( 'NONE', *, *, #11721, .F. ) ;
#9706 = CARTESIAN_POINT ( 'NONE',  ( -2.066987300000001859, 187.8999999989075036, 7.856174172912944620 ) ) ;
#9705 = PRODUCT_DEFINITION_SHAPE ( 'NONE', 'NONE',  #14597 ) ;
#9707 = AXIS2_PLACEMENT_3D ( 'NONE', #3551, #8421, #12141 ) ;
#9708 = CARTESIAN_POINT ( 'NONE',  ( 2.066987300000000527, 187.4499999989075150, 7.000000000000000000 ) ) ;
#9709 = CARTESIAN_POINT ( 'NONE',  ( -2.817313151351169775, -5.579000502529442684, 11.63234125634165927 ) ) ;
#9710 = EDGE_LOOP ( 'NONE', ( #7991, #10666 ) ) ;
#9711 = CARTESIAN_POINT ( 'NONE',  ( 3.000000000000000000, 3.673940397442059868E-16, 5.000000000000004441 ) ) ;
#9712 = ADVANCED_FACE ( 'NONE', ( #10646 ), #15090, .T. ) ;
#9713 = LINE ( 'NONE', #5010, #3998 ) ;
#9714 = PLANE ( 'NONE',  #2373 ) ;
#9715 = DIRECTION ( 'NONE',  ( 0.5877852522924802425, -0.8090169943749422332, 0.000000000000000000 ) ) ;
#9716 = CARTESIAN_POINT ( 'NONE',  ( 0.8561741729129456191, 188.3999999989075036, 4.933012699999999029 ) ) ;
#9717 = CARTESIAN_POINT ( 'NONE',  ( 4.286401442266498663, -4.198423832313231685, 18.13236078583909361 ) ) ;
#9718 = CIRCLE ( 'NONE', #1824, 12.50000000000000355 ) ;
#9719 = CARTESIAN_POINT ( 'NONE',  ( -2.500000000000000444, 1.035533905932737753, -2.249999997815050445 ) ) ;
#9720 = FACE_OUTER_BOUND ( 'NONE', #11870, .T. ) ;
#9721 = CARTESIAN_POINT ( 'NONE',  ( 5.317509234263978257, -2.779225709350955587, 31.13239388001635177 ) ) ;
#9722 = EDGE_CURVE ( 'NONE', #15372, #26, #6422, .T. ) ;
#9723 = CARTESIAN_POINT ( 'NONE',  ( -0.1323408341373540076, -6.250000000000002665, 18.99999999999998934 ) ) ;
#9724 = CARTESIAN_POINT ( 'NONE',  ( 5.935543223013847403, 0.8771126767607486663, 4.869350386511450246 ) ) ;
#9725 = CARTESIAN_POINT ( 'NONE',  ( 5.531757352715589882, 2.326874507723354579, 12.37380682714709401 ) ) ;
#9726 = EDGE_LOOP ( 'NONE', ( #9937, #13506 ) ) ;
#9727 = ORIENTED_EDGE ( 'NONE', *, *, #1324, .F. ) ;
#9728 = ORIENTED_EDGE ( 'NONE', *, *, #13196, .F. ) ;
#9729 = VECTOR ( 'NONE', #7186, 1000.000000000000114 ) ;
#9730 = CARTESIAN_POINT ( 'NONE',  ( -5.408775798201078899, -2.598833957129834005, 25.11397738943081848 ) ) ;
#9731 = ORIENTED_EDGE ( 'NONE', *, *, #6781, .T. ) ;
#9732 = CARTESIAN_POINT ( 'NONE',  ( 2.066987299999999639, 0.8561741729129456191, 1.700000001092474733 ) ) ;
#9733 = CARTESIAN_POINT ( 'NONE',  ( 0.6144377077729795689, 5.969178481556069116, 4.200339668577359298 ) ) ;
#9734 = CARTESIAN_POINT ( 'NONE',  ( 5.616116467183609018, 2.743044348085646789, 31.50425949503011225 ) ) ;
#9735 = CARTESIAN_POINT ( 'NONE',  ( 1.461580736456472573, 185.9499999989075150, 8.461580736456474128 ) ) ;
#9736 = EDGE_CURVE ( 'NONE', #1036, #1161, #7213, .T. ) ;
#9737 = CARTESIAN_POINT ( 'NONE',  ( 0.9662756667218489470, 2.500000000000000000, -2.539655916413669168 ) ) ;
#9738 = CARTESIAN_POINT ( 'NONE',  ( -1.016439536705160407E-17, 228.2551366889529731, 10.16828399152529272 ) ) ;
#9739 = CARTESIAN_POINT ( 'NONE',  ( -5.984595133899110131, -1.806709459528883288, 25.49995078984292363 ) ) ;
#9740 = CARTESIAN_POINT ( 'NONE',  ( 0.8561741729129463963, -2.066987299999999195, -2.499999998907525445 ) ) ;
#9741 = AXIS2_PLACEMENT_3D ( 'NONE', #4479, #1050, #5603 ) ;
#9742 = B_SPLINE_CURVE_WITH_KNOTS ( 'NONE', 3,
 ( #619, #12713, #1812, #5412, #10259, #11289, #386, #6684, #5256, #10103, #14957, #8918, #13752, #2860, #7708, #15662, #5958, #2047 ),
 .UNSPECIFIED., .F., .F.,
 ( 4, 2, 2, 2, 2, 2, 2, 2, 4 ),
 ( 0.003131918686235977793, 0.003523310662250268063, 0.003914702638264558332, 0.004306094614278849035, 0.004697486590293138004, 0.005088878566307427839, 0.005480270542321717675, 0.005871662518336007511, 0.006263054494350296479 ),
 .UNSPECIFIED. ) ;
#9743 = FACE_OUTER_BOUND ( 'NONE', #12738, .T. ) ;
#9744 = CARTESIAN_POINT ( 'NONE',  ( -2.257095642740105212, 226.6533546677793538, 5.453940291146690988 ) ) ;
#9745 = DIRECTION ( 'NONE',  ( -1.000000000000000000, 0.000000000000000000, 0.000000000000000000 ) ) ;
#9746 = EDGE_LOOP ( 'NONE', ( #2706, #15079, #2961, #6864 ) ) ;
#9747 = EDGE_LOOP ( 'NONE', ( #12253, #5437 ) ) ;
#9748 = ORIENTED_EDGE ( 'NONE', *, *, #9844, .T. ) ;
#9749 = EDGE_LOOP ( 'NONE', ( #12598, #1509 ) ) ;
#9750 = CARTESIAN_POINT ( 'NONE',  ( -5.558508435838179551, -2.857531096718950447, 30.86939309276501220 ) ) ;
#9751 = FACE_OUTER_BOUND ( 'NONE', #15213, .T. ) ;
#9752 = CARTESIAN_POINT ( 'NONE',  ( 1.767766952966368654, 185.5000000000000000, 8.767766952966368876 ) ) ;
#9753 = CARTESIAN_POINT ( 'NONE',  ( 4.286401442266547512, -4.198423832313182835, 11.63236078583908473 ) ) ;
#9754 = CARTESIAN_POINT ( 'NONE',  ( 4.290381260516203277, -4.545736887716273600, 23.88482219624157210 ) ) ;
#9755 = FACE_OUTER_BOUND ( 'NONE', #9383, .T. ) ;
#9756 = EDGE_CURVE ( 'NONE', #1036, #4730, #2531, .T. ) ;
#9757 = FACE_OUTER_BOUND ( 'NONE', #10569, .T. ) ;
#9758 = CARTESIAN_POINT ( 'NONE',  ( -5.570820891630690497, -2.833901239560547403, 24.23763026556123279 ) ) ;
#9759 = CARTESIAN_POINT ( 'NONE',  ( -4.435347140101107755, -4.403429997944436458, 17.99999999999998934 ) ) ;
#9760 = DIRECTION ( 'NONE',  ( 0.000000000000000000, -1.000000000000000000, 0.000000000000000000 ) ) ;
#9761 = EDGE_CURVE ( 'NONE', #546, #10381, #6962, .T. ) ;
#9762 = CARTESIAN_POINT ( 'NONE',  ( -1.767766952966369320, 188.9999999978150527, 5.232233047033630235 ) ) ;
#9763 = CARTESIAN_POINT ( 'NONE',  ( -0.1984404311693547251, 226.3267777912124075, 4.491376718485652120 ) ) ;
#9764 = CARTESIAN_POINT ( 'NONE',  ( -5.770167736194645514, -2.404664418229290224, 18.87367328635991726 ) ) ;
#9765 = AXIS2_PLACEMENT_3D ( 'NONE', #11444, #545, #13754 ) ;
#9766 = CARTESIAN_POINT ( 'NONE',  ( 5.843318061569038768, 1.367618216965670541, 31.87303779027051576 ) ) ;
#9767 = ORIENTED_EDGE ( 'NONE', *, *, #8351, .F. ) ;
#9768 = DIRECTION ( 'NONE',  ( 0.8090169943749421222, 0.5877852522924802425, 0.000000000000000000 ) ) ;
#9769 = CARTESIAN_POINT ( 'NONE',  ( 0.5044069930203958219, -5.979990686694987900, 12.37335743227902718 ) ) ;
#9770 = CARTESIAN_POINT ( 'NONE',  ( 1.035533905932737531, 2.500000000000000444, -0.9500000000000003997 ) ) ;
#9771 = DIRECTION ( 'NONE',  ( -0.000000000000000000, 1.000000000000000000, -0.000000000000000000 ) ) ;
#9772 = DIRECTION ( 'NONE',  ( -0.3090169943749446202, -0.9510565162951544194, 0.000000000000000000 ) ) ;
#9773 = LINE ( 'NONE', #212, #13513 ) ;
#9774 = CARTESIAN_POINT ( 'NONE',  ( 1.461580736456473018, -1.461580736456472573, 0.1500000010924746052 ) ) ;
#9775 = CARTESIAN_POINT ( 'NONE',  ( -3.061616997868391523E-16, 189.0000000000000000, 7.000000000000000000 ) ) ;
#9776 = DIRECTION ( 'NONE',  ( 1.000000000000000000, 0.000000000000000000, 0.000000000000000000 ) ) ;
#9777 = CARTESIAN_POINT ( 'NONE',  ( 1.767766952966368432, 188.6300000002185016, 8.767766952966368876 ) ) ;
#9778 = CARTESIAN_POINT ( 'NONE',  ( 2.500000000000000444, -1.035533905932737309, -1.849999997815050090 ) ) ;
#9779 = CARTESIAN_POINT ( 'NONE',  ( 1.974531203966234827, 228.3459296953993203, 7.238455547615789243 ) ) ;
#9780 = CARTESIAN_POINT ( 'NONE',  ( 2.066987299999999639, 0.8561741729129456191, 1.900000001092474911 ) ) ;
#9781 = CARTESIAN_POINT ( 'NONE',  ( 5.616089948629818807, -2.743103014345361856, 25.00436969680152544 ) ) ;
#9782 = ORIENTED_EDGE ( 'NONE', *, *, #10649, .F. ) ;
#9783 = CARTESIAN_POINT ( 'NONE',  ( -1.461580736456473240, 186.9499999989075150, 5.538419263543526760 ) ) ;
#9784 = CARTESIAN_POINT ( 'NONE',  ( -2.066987300000001415, 187.0999999989075206, 7.856174172912944620 ) ) ;
#9785 = CARTESIAN_POINT ( 'NONE',  ( -1.464522546803547017E-16, 2.391746824999999799, -2.562499999726881139 ) ) ;
#9787 = EDGE_LOOP ( 'NONE', ( #2962, #10690, #7835, #11866, #14865, #1603 ) ) ;
#9786 = CARTESIAN_POINT ( 'NONE',  ( 2.066987299999999639, 185.1999999989075434, 7.856174172912946396 ) ) ;
#9788 = PRESENTATION_STYLE_ASSIGNMENT (( #8521 ) ) ;
#9789 = DIRECTION ( 'NONE',  ( -1.000000000000000000, 0.000000000000000000, 0.000000000000000000 ) ) ;
#9790 = CARTESIAN_POINT ( 'NONE',  ( 5.999999999999999112, 187.2933328889893403, 9.583808270834989429 ) ) ;
#9791 = CARTESIAN_POINT ( 'NONE',  ( -0.9737725088281561359, -6.173885267451830750, 11.23735758726563994 ) ) ;
#9792 = CARTESIAN_POINT ( 'NONE',  ( -7.799024015210622274, -1.482594289697344969, 17.99999999999998934 ) ) ;
#9793 = CARTESIAN_POINT ( 'NONE',  ( -1.767766952966368432, -1.767766952966369320, -2.899999997815050357 ) ) ;
#9794 = CARTESIAN_POINT ( 'NONE',  ( -2.817313151351311884, 5.579000502529370742, 17.99999999999998934 ) ) ;
#9795 = CARTESIAN_POINT ( 'NONE',  ( -6.176542424588072677, -0.9554180641288341214, 24.49999999999999289 ) ) ;
#9796 = CARTESIAN_POINT ( 'NONE',  ( -2.931212650151679533, 5.520239928492807202, 30.49574050496989130 ) ) ;
#9797 = CARTESIAN_POINT ( 'NONE',  ( -5.615973259022320363, 2.743340227996172942, 10.99610786875028801 ) ) ;
#9798 = CARTESIAN_POINT ( 'NONE',  ( 2.848727059635853376, 5.281416301279955761, 23.88557478428062453 ) ) ;
#9799 = EDGE_CURVE ( 'NONE', #4492, #15063, #914, .T. ) ;
#9800 = ORIENTED_EDGE ( 'NONE', *, *, #9036, .T. ) ;
#9801 = EDGE_CURVE ( 'NONE', #13214, #3990, #14617, .T. ) ;
#9802 = VERTEX_POINT ( 'NONE', #13499 ) ;
#9803 = ORIENTED_EDGE ( 'NONE', *, *, #10190, .F. ) ;
#9804 = CARTESIAN_POINT ( 'NONE',  ( -1.500000000000000000, -9.750000000000003553, 0.000000000000000000 ) ) ;
#9805 = VERTEX_POINT ( 'NONE', #12152 ) ;
#9806 = CARTESIAN_POINT ( 'NONE',  ( -2.066987299999999639, 0.8561741729129452860, -1.199999998907525622 ) ) ;
#9807 = DIRECTION ( 'NONE',  ( 0.000000000000000000, 0.000000000000000000, 1.000000000000000000 ) ) ;
#9808 = AXIS2_PLACEMENT_3D ( 'NONE', #853, #5638, #6839 ) ;
#9809 = CARTESIAN_POINT ( 'NONE',  ( -1.530808498934191571E-16, 2.500000000000000000, -0.1000000000000002554 ) ) ;
#9810 = CARTESIAN_POINT ( 'NONE',  ( -0.8561741729129455081, 187.0999999989075206, 4.933012699999999029 ) ) ;
#9811 = CARTESIAN_POINT ( 'NONE',  ( -1.035533905932738197, -2.500000000000000000, -2.143000000021849871 ) ) ;
#9812 = ADVANCED_FACE ( 'NONE', ( #3480 ), #3563, .T. ) ;
#9813 = DIRECTION ( 'NONE',  ( 6.123233995736766036E-17, -1.000000000000000000, -0.000000000000000000 ) ) ;
#9814 = ITEM_DEFINED_TRANSFORMATION ( 'NONE', 'NONE', #11616,  #14201 ) ;
#9815 = CARTESIAN_POINT ( 'NONE',  ( 3.736691294293439825, 4.695920479336362696, 5.973585954366940065 ) ) ;
#9816 = CARTESIAN_POINT ( 'NONE',  ( -2.066987299999999639, 0.8561741729129452860, 1.400000001092474911 ) ) ;
#9817 = CARTESIAN_POINT ( 'NONE',  ( 2.930922878467578929, -5.520395124723519231, 4.496107868750327974 ) ) ;
#9818 = CARTESIAN_POINT ( 'NONE',  ( -2.753288529192227774, 227.6732037325579654, 8.456785184543583966 ) ) ;
#9819 = CARTESIAN_POINT ( 'NONE',  ( 5.571002711501371607, 2.833546409886354311, 5.263796168408044096 ) ) ;
#9820 = ORIENTED_EDGE ( 'NONE', *, *, #4528, .F. ) ;
#9821 = ORIENTED_EDGE ( 'NONE', *, *, #14278, .F. ) ;
#9822 = ORIENTED_EDGE ( 'NONE', *, *, #10472, .T. ) ;
#9823 = CARTESIAN_POINT ( 'NONE',  ( 5.409423237179028732, -2.597448116730994627, 30.38438267301393836 ) ) ;
#9824 = CARTESIAN_POINT ( 'NONE',  ( 2.174074108551606876, 189.0000000000000000, 5.753087109996226189 ) ) ;
#9825 = CARTESIAN_POINT ( 'NONE',  ( 1.000082492230716769, 6.169467968613709274, 5.131525381053923418 ) ) ;
#9826 = DIRECTION ( 'NONE',  ( 0.9510565162951499785, 0.3090169943749582204, 0.000000000000000000 ) ) ;
#9827 = B_SPLINE_CURVE_WITH_KNOTS ( 'NONE', 3,
 ( #12273, #3912, #13618, #12351, #3760, #6482, #3838, #12507, #10134, #11162, #8711, #8788, #2730, #9823, #7506, #262, #1445, #1373 ),
 .UNSPECIFIED., .F., .F.,
 ( 4, 2, 2, 2, 2, 2, 2, 2, 4 ),
 ( 0.003131918686235979528, 0.003523310662250269364, 0.003914702638264559199, 0.004306094614278849035, 0.004697486590293139738, 0.005088878566307429574, 0.005480270542321720277, 0.005871662518336010980, 0.006263054494350301683 ),
 .UNSPECIFIED. ) ;
#9828 = CARTESIAN_POINT ( 'NONE',  ( -1.265664690411614835E-16, 2.066987299999999639, -2.949999998907525178 ) ) ;
#9829 = LINE ( 'NONE', #11963, #8707 ) ;
#9830 = CARTESIAN_POINT ( 'NONE',  ( -6.081509788407761796, 1.446521464462625639, 5.873819640450719248 ) ) ;
#9831 = CARTESIAN_POINT ( 'NONE',  ( 0.5044069930205320462, -5.979990686694976354, 25.37335743227903251 ) ) ;
#9832 = DIRECTION ( 'NONE',  ( 0.000000000000000000, 1.000000000000000000, 0.000000000000000000 ) ) ;
#9833 = ADVANCED_FACE ( 'NONE', ( #5002 ), #11993, .F. ) ;
#9834 = CARTESIAN_POINT ( 'NONE',  ( -2.500000000000000444, 187.4499999978150981, 5.964466094067261359 ) ) ;
#9835 = CARTESIAN_POINT ( 'NONE',  ( 2.379866841847371628, 227.8775224696199473, 9.057852156131547261 ) ) ;
#9836 = CARTESIAN_POINT ( 'NONE',  ( -1.343479350821820129, 189.0800738899199018, 9.870497036542587921 ) ) ;
#9837 = EDGE_CURVE ( 'NONE', #10924, #4625, #8166, .T. ) ;
#9838 = ORIENTED_EDGE ( 'NONE', *, *, #6453, .T. ) ;
#9839 = CARTESIAN_POINT ( 'NONE',  ( -5.984595133899159869, 1.806709459528722528, 17.00004921015705861 ) ) ;
#9840 = CARTESIAN_POINT ( 'NONE',  ( -0.8730424326980312788, -5.936362132114472168, 10.99500690218562937 ) ) ;
#9841 = CARTESIAN_POINT ( 'NONE',  ( 0.000000000000000000, 184.0000000000000000, 7.000000000000000000 ) ) ;
#9842 = CARTESIAN_POINT ( 'NONE',  ( 2.817313151351171552, -5.579000502529439132, 31.13060690723500201 ) ) ;
#9843 = CARTESIAN_POINT ( 'NONE',  ( 1.933170805762127076, 226.5518075033767786, 5.154678494461841787 ) ) ;
#9844 = EDGE_CURVE ( 'NONE', #9302, #4950, #15566, .T. ) ;
#9845 = CARTESIAN_POINT ( 'NONE',  ( -2.668367453516768517, 5.373994336898062052, 11.49999999999998224 ) ) ;
#9846 = CARTESIAN_POINT ( 'NONE',  ( -2.066987299999999639, 0.000000000000000000, 1.450000001092474955 ) ) ;
#9847 = CYLINDRICAL_SURFACE ( 'NONE', #4900, 1.000000000000000666 ) ;
#9848 = DIRECTION ( 'NONE',  ( 1.000000000000000000, 0.000000000000000000, 0.000000000000000000 ) ) ;
#9849 = CARTESIAN_POINT ( 'NONE',  ( -5.570820891630792637, 2.833901239560350671, 11.76236973443871925 ) ) ;
#9850 = CARTESIAN_POINT ( 'NONE',  ( 2.500000000000000444, 186.3300000002185186, 7.000000000000000000 ) ) ;
#9851 = CARTESIAN_POINT ( 'NONE',  ( -2.500000000000000000, -1.035533905932739307, -2.149999997815051245 ) ) ;
#9852 = CIRCLE ( 'NONE', #13897, 2.499999999999999556 ) ;
#9853 = CARTESIAN_POINT ( 'NONE',  ( 0.7014106675288342974, 228.8704641679326244, 8.753341021778663134 ) ) ;
#9854 = CARTESIAN_POINT ( 'NONE',  ( -1.461580736456472351, -1.461580736456473018, -1.649999998907525356 ) ) ;
#9855 = CARTESIAN_POINT ( 'NONE',  ( 0.1323602877612372886, 6.000000000000000000, 32.00000000000000000 ) ) ;
#9856 = EDGE_LOOP ( 'NONE', ( #1335, #11214 ) ) ;
#9857 = CARTESIAN_POINT ( 'NONE',  ( -1.461580736456472795, 1.461580736456472795, 1.150000001092474688 ) ) ;
#9858 = CARTESIAN_POINT ( 'NONE',  ( -4.743384504624081899E-17, 186.8499999989074922, 4.933012699999999029 ) ) ;
#9859 = CARTESIAN_POINT ( 'NONE',  ( -3.781065399485981526, -4.978303713186466695, 12.49991741810287316 ) ) ;
#9860 =( NAMED_UNIT ( * ) SI_UNIT ( $, .STERADIAN. ) SOLID_ANGLE_UNIT ( ) );
#9862 = ORIENTED_EDGE ( 'NONE', *, *, #5612, .F. ) ;
#9861 = CARTESIAN_POINT ( 'NONE',  ( 3.158296126777810464, 5.394094919772101981, 30.20112161576661336 ) ) ;
#9863 =( NAMED_UNIT ( * ) SI_UNIT ( $, .STERADIAN. ) SOLID_ANGLE_UNIT ( ) );
#9864 = AXIS2_PLACEMENT_3D ( 'NONE', #12083, #1182, #10898 ) ;
#9865 = CARTESIAN_POINT ( 'NONE',  ( 0.9740856415302890925, -6.173834621338562201, 24.23852653055532258 ) ) ;
#9866 = DIRECTION ( 'NONE',  ( -1.000000000000000000, -6.123233995736766036E-17, 0.000000000000000000 ) ) ;
#9867 = CARTESIAN_POINT ( 'NONE',  ( 0.1323408341374891495, 6.250000000000001776, 12.49999999999999289 ) ) ;
#9868 = CARTESIAN_POINT ( 'NONE',  ( -1.382083006809480485, 189.0000000000000000, 9.086164795105178271 ) ) ;
#9869 = CARTESIAN_POINT ( 'NONE',  ( 5.620786884546368434, -2.102685372472677727, 25.47358595436692852 ) ) ;
#9870 = DIRECTION ( 'NONE',  ( -6.123233995736766036E-17, 1.000000000000000000, 0.000000000000000000 ) ) ;
#9871 = CARTESIAN_POINT ( 'NONE',  ( -0.5042987395407539930, -5.979983180450077818, 31.87329304179976930 ) ) ;
#9872 = CARTESIAN_POINT ( 'NONE',  ( 5.531796221294883686, -2.326749136277200147, 31.87378430870261425 ) ) ;
#9874 = CARTESIAN_POINT ( 'NONE',  ( -3.255013540813658679, 5.336859797930821436, 30.12618035954927009 ) ) ;
#9873 = VECTOR ( 'NONE', #3892, 1000.000000000000114 ) ;
#9875 = DIRECTION ( 'NONE',  ( 0.000000000000000000, 0.000000000000000000, -1.000000000000000000 ) ) ;
#9876 = CARTESIAN_POINT ( 'NONE',  ( 2.897581130414634077E-17, -9.750000000000003553, 2.000000000000001776 ) ) ;
#9877 = ORIENTED_EDGE ( 'NONE', *, *, #11085, .T. ) ;
#9878 = EDGE_LOOP ( 'NONE', ( #12432, #4748 ) ) ;
#9879 = VERTEX_POINT ( 'NONE', #2999 ) ;
#9880 = CARTESIAN_POINT ( 'NONE',  ( -3.107688324358885090, 5.133887830459729962, 25.37378430870261781 ) ) ;
#9881 = ORIENTED_EDGE ( 'NONE', *, *, #12792, .F. ) ;
#9882 = AXIS2_PLACEMENT_3D ( 'NONE', #1120, #3271, #2147 ) ;
#9883 = CARTESIAN_POINT ( 'NONE',  ( -0.8561741729129458411, -2.066987299999999195, -0.1999999989075254836 ) ) ;
#9884 = AXIS2_PLACEMENT_3D ( 'NONE', #4071, #3754, #8629 ) ;
#9885 = FACE_OUTER_BOUND ( 'NONE', #4096, .T. ) ;
#9886 = DIRECTION ( 'NONE',  ( 0.9510565162951500895, 0.3090169943749582204, 0.000000000000000000 ) ) ;
#9887 = FACE_OUTER_BOUND ( 'NONE', #7521, .T. ) ;
#9888 = CARTESIAN_POINT ( 'NONE',  ( -2.500000000000000000, -1.035533905932739307, 1.750000000000000222 ) ) ;
#9889 = EDGE_CURVE ( 'NONE', #471, #15059, #14405, .T. ) ;
#9890 = DIRECTION ( 'NONE',  ( 0.000000000000000000, 1.000000000000000000, 0.000000000000000000 ) ) ;
#9891 = CYLINDRICAL_SURFACE ( 'NONE', #4187, 1.000000000000000666 ) ;
#9892 = CARTESIAN_POINT ( 'NONE',  ( -2.066987299999999639, 0.8561741729129452860, -1.999999998907524779 ) ) ;
#9893 = CARTESIAN_POINT ( 'NONE',  ( 5.985119669071130133, -1.805077827356517117, 10.50008258189709132 ) ) ;
#9894 = CARTESIAN_POINT ( 'NONE',  ( -2.599074790483714370, 227.7726799100639994, 8.749447567440038043 ) ) ;
#9895 = ORIENTED_EDGE ( 'NONE', *, *, #7884, .T. ) ;
#9896 = AXIS2_PLACEMENT_3D ( 'NONE', #6771, #13093, #11450 ) ;
#9897 = EDGE_LOOP ( 'NONE', ( #6423, #3776, #12040, #3023 ) ) ;
#9898 = ORIENTED_EDGE ( 'NONE', *, *, #14283, .F. ) ;
#9899 = DIRECTION ( 'NONE',  ( -0.3090169943749584425, 0.9510565162951498674, 0.000000000000000000 ) ) ;
#9900 = CARTESIAN_POINT ( 'NONE',  ( 0.5022380396211999498, 188.9999999999999716, 9.452991705245926468 ) ) ;
#9901 = CARTESIAN_POINT ( 'NONE',  ( -5.725684683139550479, -2.507514573674904934, 17.20112161576660981 ) ) ;
#9902 = CARTESIAN_POINT ( 'NONE',  ( 0.1323933160975826473, -5.999999999999999112, 32.00000000000000000 ) ) ;
#9903 = EDGE_CURVE ( 'NONE', #12866, #12482, #12130, .T. ) ;
#9904 = PLANE ( 'NONE',  #14935 ) ;
#9905 = CARTESIAN_POINT ( 'NONE',  ( 1.767766952966369320, 185.5999999978150754, 5.232233047033630235 ) ) ;
#9906 = CARTESIAN_POINT ( 'NONE',  ( 9.750000000000003553, 22.00000000000000000, -1.499999999999897415 ) ) ;
#9907 = CARTESIAN_POINT ( 'NONE',  ( 5.317509234264001350, -2.779225709350913398, 11.63239388001634289 ) ) ;
#9908 = CARTESIAN_POINT ( 'NONE',  ( -2.817313151351312328, 5.579000502529370742, 18.13237410716305220 ) ) ;
#9909 = DIRECTION ( 'NONE',  ( -1.000000000000000000, 0.000000000000000000, 0.000000000000000000 ) ) ;
#9910 = CARTESIAN_POINT ( 'NONE',  ( -1.767766952966369542, 185.2699999975965568, 8.767766952966368876 ) ) ;
#9911 = CARTESIAN_POINT ( 'NONE',  ( -1.385362557672197736, 227.7924883072852822, 5.640085252515396164 ) ) ;
#9912 = EDGE_CURVE ( 'NONE', #4153, #478, #8542, .T. ) ;
#9913 = CARTESIAN_POINT ( 'NONE',  ( 2.807343268925317492, 227.6302376672054208, 8.330365510804844220 ) ) ;
#9914 = CARTESIAN_POINT ( 'NONE',  ( -0.07717340183324516989, 189.6978550888158850, 10.38866401756452262 ) ) ;
#9915 =( GEOMETRIC_REPRESENTATION_CONTEXT ( 3 ) GLOBAL_UNCERTAINTY_ASSIGNED_CONTEXT ( ( #11660 ) ) GLOBAL_UNIT_ASSIGNED_CONTEXT ( ( #1945, #9434, #7131 ) ) REPRESENTATION_CONTEXT ( 'NONE', 'WORKASPACE' ) );
#9916 = ORIENTED_EDGE ( 'NONE', *, *, #9248, .F. ) ;
#9917 = CARTESIAN_POINT ( 'NONE',  ( 0.000000000000000000, 0.000000000000000000, 0.000000000000000000 ) ) ;
#9918 = CARTESIAN_POINT ( 'NONE',  ( -5.726307184802593930, 2.506131700382597582, 23.69973484982322987 ) ) ;
#9919 = CARTESIAN_POINT ( 'NONE',  ( 0.6151877315910523336, -6.220340188096010081, 12.29906673469668021 ) ) ;
#9920 = CARTESIAN_POINT ( 'NONE',  ( 1.734723475976807094E-15, 2.000000000000000000, 13.50000000000000000 ) ) ;
#9921 = CARTESIAN_POINT ( 'NONE',  ( 2.771580177427784619, 226.9203070754519729, 6.240395558440384960 ) ) ;
#9922 = CARTESIAN_POINT ( 'NONE',  ( 3.882809187878787593, 4.899079348630168695, 23.52599901976669727 ) ) ;
#9923 = CARTESIAN_POINT ( 'NONE',  ( 2.500000000000000444, 1.035533905932737975, 2.149999999999999911 ) ) ;
#9924 = CARTESIAN_POINT ( 'NONE',  ( 5.940390500375550609, 6.474944468551622201, 5.000000000000004441 ) ) ;
#9925 = SURFACE_SIDE_STYLE ('',( #4840 ) ) ;
#9926 = EDGE_CURVE ( 'NONE', #302, #9042, #10018, .T. ) ;
#9927 = CARTESIAN_POINT ( 'NONE',  ( -1.500000000000000000, 0.000000000000000000, 2.500000000000000000 ) ) ;
#9928 = CARTESIAN_POINT ( 'NONE',  ( 1.767766952966369098, 187.2300000002184959, 5.232233047033630235 ) ) ;
#9929 = CARTESIAN_POINT ( 'NONE',  ( 2.500000000000000000, 3.061616997868383141E-16, -1.799999997815050490 ) ) ;
#9930 = CARTESIAN_POINT ( 'NONE',  ( 1.360905158423219241, 228.7363411735375962, 8.365986164091459898 ) ) ;
#9931 = CARTESIAN_POINT ( 'NONE',  ( -2.066987299999999639, 0.000000000000000000, -1.749999998907525223 ) ) ;
#9932 = CARTESIAN_POINT ( 'NONE',  ( 4.153663429050711287, 4.670992970568434544, 12.29933148907576346 ) ) ;
#9933 = CARTESIAN_POINT ( 'NONE',  ( -0.8561741729129458411, -2.066987299999999195, 1.400000001092474911 ) ) ;
#9934 = CARTESIAN_POINT ( 'NONE',  ( -2.066987300000001859, 188.6999999989075150, 7.856174172912944620 ) ) ;
#9935 = CARTESIAN_POINT ( 'NONE',  ( 2.500000000000000444, 187.0999999978150754, 7.000000000000000000 ) ) ;
#9937 = ORIENTED_EDGE ( 'NONE', *, *, #460, .F. ) ;
#9936 = CARTESIAN_POINT ( 'NONE',  ( 2.066987300000000083, 186.0499999989075093, 7.000000000000000000 ) ) ;
#9938 = AXIS2_PLACEMENT_3D ( 'NONE', #10951, #10873, #12640 ) ;
#9939 = CARTESIAN_POINT ( 'NONE',  ( -2.849269941562089681, -5.281123252783978650, 23.88480617551149265 ) ) ;
#9940 = DIRECTION ( 'NONE',  ( 0.8090169943749421222, 0.5877852522924802425, 0.000000000000000000 ) ) ;
#9942 = CARTESIAN_POINT ( 'NONE',  ( -9.750000000000003553, 184.0000000000000000, 1.499999999999965583 ) ) ;
#9941 = B_SPLINE_CURVE_WITH_KNOTS ( 'NONE', 3,
 ( #13216, #8377, #10672, #881, #11778, #7259, #13050, #15689, #10591, #10827, #4554, #12970, #2309, #4791, #4711, #2229, #15530, #5905, #14238, #9323, #15453, #12096, #13128, #15610 ),
 .UNSPECIFIED., .F., .F.,
 ( 4, 2, 2, 2, 2, 2, 2, 2, 2, 2, 2, 4 ),
 ( 0.000000000000000000, 0.06249999999999945877, 0.1249999999999989175, 0.1562499999999986400, 0.1874999999999983902, 0.2499999999999993339, 0.3125000000000002776, 0.3437500000000007216, 0.3750000000000011657, 0.4375000000000006661, 0.4687500000000003331, 0.5000000000000000000 ),
 .UNSPECIFIED. ) ;
#9943 = CARTESIAN_POINT ( 'NONE',  ( -5.621278735166254314, 2.101423246382402521, 4.025919472168996371 ) ) ;
#9944 = CARTESIAN_POINT ( 'NONE',  ( -0.9740012993919509032, -6.173846968979653127, 11.76164920628437649 ) ) ;
#9945 = CARTESIAN_POINT ( 'NONE',  ( -1.767766952966368432, -1.767766952966369320, 0.2000000000000000944 ) ) ;
#9946 = CARTESIAN_POINT ( 'NONE',  ( 1.035533905932739085, -2.500000000000000000, -2.749999997815050445 ) ) ;
#9947 = CARTESIAN_POINT ( 'NONE',  ( -2.897581130414634077E-17, 19.99999999999999645, -9.750000000000003553 ) ) ;
#9948 = CARTESIAN_POINT ( 'NONE',  ( 2.656575965584776711, 189.9553606806719017, 5.797866007794856280 ) ) ;
#9949 = CARTESIAN_POINT ( 'NONE',  ( -0.6156133477425491662, -6.220296490279956458, 18.79872387345510276 ) ) ;
#9950 = EDGE_CURVE ( 'NONE', #4648, #6307, #8092, .T. ) ;
#9951 = CARTESIAN_POINT ( 'NONE',  ( -5.531623157106135835, -2.327208526676509237, 12.37364704684421568 ) ) ;
#9952 = CARTESIAN_POINT ( 'NONE',  ( 5.330189595673637371, 2.755293208590243292, 11.76382603205595956 ) ) ;
#9953 = ORIENTED_EDGE ( 'NONE', *, *, #3508, .T. ) ;
#9954 = CARTESIAN_POINT ( 'NONE',  ( -5.421010862427522170E-16, 186.6499999989075320, 9.066987300000000971 ) ) ;
#9955 = VERTEX_POINT ( 'NONE', #2030 ) ;
#9956 = DIRECTION ( 'NONE',  ( 0.000000000000000000, 0.000000000000000000, 1.000000000000000000 ) ) ;
#9957 = EDGE_LOOP ( 'NONE', ( #10149, #162, #5022, #10281 ) ) ;
#9958 = CARTESIAN_POINT ( 'NONE',  ( -3.922672396097227399, 4.541739265057554320, 25.37364704684422634 ) ) ;
#9959 = EDGE_LOOP ( 'NONE', ( #551, #3522, #6621, #10170 ) ) ;
#9960 = AXIS2_PLACEMENT_3D ( 'NONE', #4579, #7045, #9430 ) ;
#9961 = CARTESIAN_POINT ( 'NONE',  ( 1.461580736456472573, 1.461580736456472795, 0.1500000010924747995 ) ) ;
#9962 = CARTESIAN_POINT ( 'NONE',  ( 5.616116467183658756, 2.743044348085541539, 18.50425949503010159 ) ) ;
#9963 = CARTESIAN_POINT ( 'NONE',  ( -1.126573280235289021, 228.1844602338491370, 9.960491586248465978 ) ) ;
#9964 = CARTESIAN_POINT ( 'NONE',  ( 0.000000000000000000, 0.000000000000000000, 0.000000000000000000 ) ) ;
#9965 = CARTESIAN_POINT ( 'NONE',  ( 4.592425496802573972E-16, -2.500000000000000000, 1.899999999999999911 ) ) ;
#9966 = FACE_BOUND ( 'NONE', #1679, .T. ) ;
#9967 = EDGE_CURVE ( 'NONE', #3666, #5746, #4156, .T. ) ;
#9968 = ITEM_DEFINED_TRANSFORMATION ( 'NONE', 'NONE', #7558,  #14201 ) ;
#9969 = CARTESIAN_POINT ( 'NONE',  ( 2.668367453516689469, -5.373994336898103796, 31.13061695532139339 ) ) ;
#9970 = CARTESIAN_POINT ( 'NONE',  ( 1.461580736456472573, 1.461580736456472795, -0.4499999989075252338 ) ) ;
#9971 = CARTESIAN_POINT ( 'NONE',  ( 6.172614129015244977, -0.9817721000788082186, 11.23763026556121503 ) ) ;
#9972 = CARTESIAN_POINT ( 'NONE',  ( -2.051698115976866355, 227.9946287341323057, 9.402281653761695779 ) ) ;
#9973 = EDGE_LOOP ( 'NONE', ( #5197, #9663 ) ) ;
#9974 = VERTEX_POINT ( 'NONE', #841 ) ;
#9975 = ORIENTED_EDGE ( 'NONE', *, *, #9136, .F. ) ;
#9976 = CARTESIAN_POINT ( 'NONE',  ( 0.6144377077731314474, 5.969178481556053129, 17.20033966857735663 ) ) ;
#9977 = CARTESIAN_POINT ( 'NONE',  ( 0.9656511469083723931, 188.9999999999999716, 4.686691486504618531 ) ) ;
#9978 = ORIENTED_EDGE ( 'NONE', *, *, #14202, .F. ) ;
#9979 = CARTESIAN_POINT ( 'NONE',  ( 0.000000000000000000, 6.250000000000000888, 6.000000000000005329 ) ) ;
#9980 = CARTESIAN_POINT ( 'NONE',  ( -4.286401442266626560, -4.198423832313095794, 18.13061695532137207 ) ) ;
#9981 = B_SPLINE_CURVE_WITH_KNOTS ( 'NONE', 3,
 ( #11726, #8078, #14188, #12919, #10540, #3065, #15398, #4493, #9348, #2096, #15478, #14261, #12758, #3371, #8238, #11569, #10933, #13154 ),
 .UNSPECIFIED., .F., .F.,
 ( 4, 2, 2, 2, 2, 2, 2, 2, 4 ),
 ( 0.000000000000000000, 0.0003914898357794974410, 0.0007829796715589948820, 0.001174469507338492215, 0.001565959343117989764, 0.001957449178897485795, 0.002348939014676982261, 0.002740428850456478726, 0.003131918686235975191 ),
 .UNSPECIFIED. ) ;
#9982 = CARTESIAN_POINT ( 'NONE',  ( 2.930922878467408843, -5.520395124723609825, 23.99610786875029333 ) ) ;
#9983 = CARTESIAN_POINT ( 'NONE',  ( 0.6144300524835216715, 6.220417338033038313, 17.20033372175934616 ) ) ;
#9984 = CARTESIAN_POINT ( 'NONE',  ( -1.767766952966369765, 187.5999999978150754, 8.767766952966368876 ) ) ;
#9985 = VECTOR ( 'NONE', #11945, 1000.000000000000114 ) ;
#9986 = CARTESIAN_POINT ( 'NONE',  ( -6.172552660730998397, 0.9821660343537570448, 5.263796168408045872 ) ) ;
#9987 = CARTESIAN_POINT ( 'NONE',  ( 0.6139908388542947293, -5.969238533166593363, 23.69977627912011897 ) ) ;
#9988 = CARTESIAN_POINT ( 'NONE',  ( 0.000000000000000000, 104.0000000000000142, 0.000000000000000000 ) ) ;
#9989 = CARTESIAN_POINT ( 'NONE',  ( 2.500000000000000444, 185.6199999975965795, 5.964466094067262247 ) ) ;
#9990 = CARTESIAN_POINT ( 'NONE',  ( 0.5489208960863538600, 227.6341400683239726, 5.182766506802777506 ) ) ;
#9991 = CARTESIAN_POINT ( 'NONE',  ( -2.257704606524308488, 227.9260547655458140, 9.200601119324863575 ) ) ;
#9992 = EDGE_CURVE ( 'NONE', #1161, #11432, #5706, .T. ) ;
#9993 = CARTESIAN_POINT ( 'NONE',  ( -2.877165451417496023, 189.2399726852219715, 8.034986858290199763 ) ) ;
#9994 = AXIS2_PLACEMENT_3D ( 'NONE', #6493, #4004, #10143 ) ;
#9995 = ORIENTED_EDGE ( 'NONE', *, *, #4632, .T. ) ;
#9996 = EDGE_CURVE ( 'NONE', #4594, #2495, #15350, .T. ) ;
#9997 = CARTESIAN_POINT ( 'NONE',  ( 9.750000000000003553, -1.020968533498575335E-13, 2.000000000000001776 ) ) ;
#9998 = CARTESIAN_POINT ( 'NONE',  ( 2.840966774240241577, -5.567223638426863630, 11.23809786915986741 ) ) ;
#9999 = CARTESIAN_POINT ( 'NONE',  ( -3.634089073485594401, 4.776071126502567488, 23.50007997643738378 ) ) ;
#10000 = CARTESIAN_POINT ( 'NONE',  ( 5.616089948629698014, 2.743103014345608326, 30.49563030319847101 ) ) ;
#10001 = CARTESIAN_POINT ( 'NONE',  ( 1.974191107854609495, 228.0195094073193331, 9.475456042165514958 ) ) ;
#10002 = EDGE_CURVE ( 'NONE', #4668, #7716, #12492, .T. ) ;
#10003 = CARTESIAN_POINT ( 'NONE',  ( 4.195842658231396349, -4.289229542213240265, 23.99560239355786351 ) ) ;
#10004 = CARTESIAN_POINT ( 'NONE',  ( -1.035533905932737753, 2.500000000000000444, 1.550000000000000044 ) ) ;
#10005 = CARTESIAN_POINT ( 'NONE',  ( 5.935543223013858949, -0.8771126767606638452, 5.000000000000004441 ) ) ;
#10006 = SURFACE_SIDE_STYLE ('',( #2759 ) ) ;
#10007 = LINE ( 'NONE', #13882, #7730 ) ;
#10008 = CARTESIAN_POINT ( 'NONE',  ( -2.500000000000000444, 186.8499999999999943, 8.035533905932737753 ) ) ;
#10009 = FACE_BOUND ( 'NONE', #7875, .T. ) ;
#10010 = CARTESIAN_POINT ( 'NONE',  ( -1.212146835196386663, 227.7435586823976337, 5.498773705076675178 ) ) ;
#10011 = CARTESIAN_POINT ( 'NONE',  ( 0.8561741729129465073, -2.066987299999999195, -1.499999998907525445 ) ) ;
#10012 = CARTESIAN_POINT ( 'NONE',  ( 4.069684453406249958, 4.744965295353598123, 12.37380055247394672 ) ) ;
#10013 = CARTESIAN_POINT ( 'NONE',  ( -2.066987299999999195, -0.8561741729129467293, 1.300000001092474600 ) ) ;
#10014 = CARTESIAN_POINT ( 'NONE',  ( 1.767766952966369320, 184.0999999999999943, 5.232233047033630235 ) ) ;
#10015 = CARTESIAN_POINT ( 'NONE',  ( 6.143143148203078496, -1.154591847827606488, 18.61396179408071205 ) ) ;
#10017 = EDGE_LOOP ( 'NONE', ( #5882, #9023, #1273 ) ) ;
#10016 = CARTESIAN_POINT ( 'NONE',  ( 1.461580736456472351, 187.5499999989075093, 8.461580736456474128 ) ) ;
#10018 = CIRCLE ( 'NONE', #9244, 1.999999999999999556 ) ;
#10019 = DIRECTION ( 'NONE',  ( 0.000000000000000000, 0.000000000000000000, 1.000000000000000000 ) ) ;
#10020 = CARTESIAN_POINT ( 'NONE',  ( 5.725930890718349708, -2.506952462184002250, 12.29933148907576523 ) ) ;
#10021 = CARTESIAN_POINT ( 'NONE',  ( 6.780834054130108014E-14, -6.250000000000000888, 10.49999999999998224 ) ) ;
#10022 = CARTESIAN_POINT ( 'NONE',  ( 4.141923667210556381, 4.342011609040548947, 17.38438267301393481 ) ) ;
#10023 = CARTESIAN_POINT ( 'NONE',  ( 2.174074109817228706, 188.9999999993558504, 5.753087114337779973 ) ) ;
#10024 = CARTESIAN_POINT ( 'NONE',  ( -1.294371610423890733E-14, -0.3999999999999905853, -2.454447735324990276 ) ) ;
#10025 = CARTESIAN_POINT ( 'NONE',  ( 1.840960705394127928, 189.7476812664443742, 9.752039420742224962 ) ) ;
#10026 = CARTESIAN_POINT ( 'NONE',  ( -5.487348639458876853, 2.428538342494443114, 10.69977782616119732 ) ) ;
#10027 = CARTESIAN_POINT ( 'NONE',  ( -5.487348639458853761, -2.428538342494495961, 12.30022217383879202 ) ) ;
#10028 = EDGE_CURVE ( 'NONE', #12110, #11794, #14536, .T. ) ;
#10029 = CARTESIAN_POINT ( 'NONE',  ( -0.6508408531687689402, 189.0000000000000000, 4.580680803288122327 ) ) ;
#10030 = ORIENTED_EDGE ( 'NONE', *, *, #9761, .T. ) ;
#10031 = CARTESIAN_POINT ( 'NONE',  ( 1.461580736456472795, 186.9499999989075150, 5.538419263543527649 ) ) ;
#10032 = ORIENTED_EDGE ( 'NONE', *, *, #7354, .T. ) ;
#10033 = CARTESIAN_POINT ( 'NONE',  ( -5.531209434046251872, -2.328189801702823303, 23.62696220972947359 ) ) ;
#10034 = VECTOR ( 'NONE', #15016, 1000.000000000000000 ) ;
#10035 = EDGE_LOOP ( 'NONE', ( #2275, #13523, #1060, #1932 ) ) ;
#10036 = EDGE_CURVE ( 'NONE', #14984, #15527, #11926, .T. ) ;
#10037 = CARTESIAN_POINT ( 'NONE',  ( -5.783239563508360881, -1.602707436861348311, 25.47358595436692852 ) ) ;
#10038 = VERTEX_POINT ( 'NONE', #11473 ) ;
#10039 = CARTESIAN_POINT ( 'NONE',  ( 3.796994071234844259E-16, -2.066987299999999639, -0.9499999989075252893 ) ) ;
#10040 = CARTESIAN_POINT ( 'NONE',  ( -3.255013540813639139, 5.336859797930833871, 4.126180359549289633 ) ) ;
#10041 = CARTESIAN_POINT ( 'NONE',  ( -1.991442181821953650, 228.0119299072603383, 9.453167579138481713 ) ) ;
#10042 = CYLINDRICAL_SURFACE ( 'NONE', #2323, 1.000000000000000888 ) ;
#10043 = CARTESIAN_POINT ( 'NONE',  ( 1.767766952966368654, 1.767766952966369098, 2.200000000000000178 ) ) ;
#10044 = AXIS2_PLACEMENT_3D ( 'NONE', #12658, #7727, #10434 ) ;
#10045 = FACE_OUTER_BOUND ( 'NONE', #8129, .T. ) ;
#10046 = ITEM_DEFINED_TRANSFORMATION ( 'NONE', 'NONE', #9104,  #14201 ) ;
#10047 = CARTESIAN_POINT ( 'NONE',  ( 2.692335458626958999, -5.362264153667180011, 31.26239891805598248 ) ) ;
#10048 = CARTESIAN_POINT ( 'NONE',  ( 2.066987300000000083, -0.8561741729129449530, -0.5999999989075250895 ) ) ;
#10049 = DIRECTION ( 'NONE',  ( 0.000000000000000000, 0.000000000000000000, 1.000000000000000000 ) ) ;
#10050 = CARTESIAN_POINT ( 'NONE',  ( 3.312524433819759917, 5.004191858254014136, 12.47408052783098853 ) ) ;
#10051 = VERTEX_POINT ( 'NONE', #1613 ) ;
#10052 = ORIENTED_EDGE ( 'NONE', *, *, #2821, .F. ) ;
#10053 = ORIENTED_EDGE ( 'NONE', *, *, #2416, .T. ) ;
#10054 = CARTESIAN_POINT ( 'NONE',  ( 1.353717517954364224E-13, 6.000000000000000888, 18.99999999999998934 ) ) ;
#10055 = CARTESIAN_POINT ( 'NONE',  ( 3.458623254138723624, 5.207221900902812450, 4.026227171247320769 ) ) ;
#10056 = ORIENTED_EDGE ( 'NONE', *, *, #3583, .T. ) ;
#10057 = AXIS2_PLACEMENT_3D ( 'NONE', #13395, #11090, #12203 ) ;
#10058 = CARTESIAN_POINT ( 'NONE',  ( -6.176542424588085112, -0.9554180641287668418, 17.86765874365829632 ) ) ;
#10059 = CARTESIAN_POINT ( 'NONE',  ( 0.5039079366032624963, -5.980031194523149907, 30.12637068109813043 ) ) ;
#10060 = CARTESIAN_POINT ( 'NONE',  ( -3.779082820360686323, 4.979770177899256467, 32.00004906876533539 ) ) ;
#10061 = CARTESIAN_POINT ( 'NONE',  ( -2.500000000000000444, 187.4999999978150527, 7.000000000000000000 ) ) ;
#10062 = CARTESIAN_POINT ( 'NONE',  ( -2.500000000000000444, 185.9499999978150413, 8.035533905932737753 ) ) ;
#10063 = DIRECTION ( 'NONE',  ( 1.000000000000000000, 0.000000000000000000, 0.000000000000000000 ) ) ;
#10064 = DIRECTION ( 'NONE',  ( -1.000000000000000000, 0.000000000000000000, 0.000000000000000000 ) ) ;
#10065 = CYLINDRICAL_SURFACE ( 'NONE', #1587, 1.000000000000000666 ) ;
#10066 = DIRECTION ( 'NONE',  ( 1.000000000000000000, 0.000000000000000000, 0.000000000000000000 ) ) ;
#10067 = CARTESIAN_POINT ( 'NONE',  ( 1.035533905932737753, 187.3199999975965966, 4.500000000000000888 ) ) ;
#10068 = CARTESIAN_POINT ( 'NONE',  ( -1.938951794131667850, 228.1124887269953092, 6.564264716264994526 ) ) ;
#10069 = CARTESIAN_POINT ( 'NONE',  ( -2.052299789776659722, 226.5858468330626465, 5.255005641065958244 ) ) ;
#10070 = CARTESIAN_POINT ( 'NONE',  ( -0.7435873775819946685, 188.9999999999307931, 9.391030955749405607 ) ) ;
#10071 = ORIENTED_EDGE ( 'NONE', *, *, #12700, .T. ) ;
#10072 = CARTESIAN_POINT ( 'NONE',  ( -5.570722351696237418, 2.834100162822021929, 17.73809786915987274 ) ) ;
#10073 = CARTESIAN_POINT ( 'NONE',  ( 4.069684453406335223, -4.744965295353526180, 10.62619944752603374 ) ) ;
#10074 = CARTESIAN_POINT ( 'NONE',  ( -0.9999505860953411540, 6.169489349035806924, 5.131059031658106839 ) ) ;
#10075 = CARTESIAN_POINT ( 'NONE',  ( 6.176542424588115310, 0.9554180641285648923, 11.49999999999998224 ) ) ;
#10076 = CARTESIAN_POINT ( 'NONE',  ( 2.814970402829801710, 226.9540368158492925, 6.339744779883301540 ) ) ;
#10077 = CARTESIAN_POINT ( 'NONE',  ( 4.005998022989880170, -4.467726698309333777, 23.70068193741825624 ) ) ;
#10078 = CARTESIAN_POINT ( 'NONE',  ( 2.500000000000000444, -1.035533905932737309, 2.049999999999999822 ) ) ;
#10079 = DIRECTION ( 'NONE',  ( 0.5877852522924802425, -0.8090169943749422332, 0.000000000000000000 ) ) ;
#10080 = CARTESIAN_POINT ( 'NONE',  ( -3.158825713737467122, -5.393784879207181859, 30.20066851092422411 ) ) ;
#10081 =( BOUNDED_CURVE ( )  B_SPLINE_CURVE ( 2, ( #5741, #11697, #10662, #4704, #3414, #8125, #15682, #6938, #2302 ),
 .UNSPECIFIED., .F., .F. ) 
 B_SPLINE_CURVE_WITH_KNOTS ( ( 3, 2, 2, 2, 3 ),
 ( 0.7142857142857143016, 0.7321428571428570953, 0.7500000000000000000, 0.7678571428571429047, 0.7678695020645334157 ),
 .UNSPECIFIED. ) 
 CURVE ( )  GEOMETRIC_REPRESENTATION_ITEM ( )  RATIONAL_B_SPLINE_CURVE ( ( 1.000000000000000000, 0.9238795325112867385, 1.000000000000000000, 0.9238795325112867385, 1.000000000000000000, 0.9238795325112867385, 1.000000000000000000, 0.9999473158359161173, 0.9998947045988972882 ) ) 
 REPRESENTATION_ITEM ( '' )  );
#10082 = CARTESIAN_POINT ( 'NONE',  ( 1.767766952966368432, 187.0999999999999943, 8.767766952966368876 ) ) ;
#10083 = FACE_BOUND ( 'NONE', #15591, .T. ) ;
#10084 = ADVANCED_FACE ( 'NONE', ( #13785 ), #10292, .T. ) ;
#10085 = CARTESIAN_POINT ( 'NONE',  ( -1.132970084112051579, 227.7246690377758398, 5.444219334014433365 ) ) ;
#10086 = CARTESIAN_POINT ( 'NONE',  ( -1.965116437629976787E-16, 189.2499999989075263, 4.933012699999999029 ) ) ;
#10087 = CARTESIAN_POINT ( 'NONE',  ( -2.500000000000000444, 1.035533905932737753, -3.049999997815050268 ) ) ;
#10088 = FACE_OUTER_BOUND ( 'NONE', #11279, .T. ) ;
#10089 = CARTESIAN_POINT ( 'NONE',  ( 2.066987299999999639, 188.1999999989075150, 7.856174172912946396 ) ) ;
#10090 = CARTESIAN_POINT ( 'NONE',  ( 5.903596343266337421, -2.055998103990466230, 18.99995078984292007 ) ) ;
#10092 = ORIENTED_EDGE ( 'NONE', *, *, #5848, .T. ) ;
#10091 = CARTESIAN_POINT ( 'NONE',  ( -0.8561741729129456191, 187.8999999989075320, 4.933012699999999029 ) ) ;
#10093 = DIRECTION ( 'NONE',  ( 0.9510565162951500895, 0.3090169943749582204, 0.000000000000000000 ) ) ;
#10094 = EDGE_CURVE ( 'NONE', #13484, #3329, #14963, .T. ) ;
#10095 = CARTESIAN_POINT ( 'NONE',  ( 6.176542424588130409, -0.9554180641284772957, 11.63063932754212892 ) ) ;
#10096 = CARTESIAN_POINT ( 'NONE',  ( 0.000000000000000000, 201.6409668649146738, 13.30942870683726298 ) ) ;
#10097 = EDGE_CURVE ( 'NONE', #338, #10381, #7027, .T. ) ;
#10098 = DIRECTION ( 'NONE',  ( 0.000000000000000000, 1.000000000000000000, 0.000000000000000000 ) ) ;
#10099 = CARTESIAN_POINT ( 'NONE',  ( 2.848727059635912884, 5.281416301279922898, 17.38557478428061387 ) ) ;
#10100 = CARTESIAN_POINT ( 'NONE',  ( 2.328196544915174027, 189.0000000006442065, 6.072157968082956714 ) ) ;
#10101 = DIRECTION ( 'NONE',  ( -0.9510565162951544194, 0.3090169943749447312, 0.000000000000000000 ) ) ;
#10102 = CARTESIAN_POINT ( 'NONE',  ( 3.010624175978056538, -5.190832888732173522, 5.798882422479413101 ) ) ;
#10103 = CARTESIAN_POINT ( 'NONE',  ( -3.420311045507836045, 4.931422832349298346, 29.99992038825523011 ) ) ;
#10104 = CARTESIAN_POINT ( 'NONE',  ( 2.500000000000000444, 184.3499999989075206, 7.000000000000000000 ) ) ;
#10105 = CYLINDRICAL_SURFACE ( 'NONE', #8749, 5.000000000000000000 ) ;
#10106 = EDGE_LOOP ( 'NONE', ( #378, #13928, #7278, #5649 ) ) ;
#10107 = CARTESIAN_POINT ( 'NONE',  ( 0.8561741729129455081, 186.1999999989075150, 4.933012699999999029 ) ) ;
#10108 = AXIS2_PLACEMENT_3D ( 'NONE', #4087, #1542, #10066 ) ;
#10109 = ORIENTED_EDGE ( 'NONE', *, *, #6800, .T. ) ;
#10110 = CARTESIAN_POINT ( 'NONE',  ( 0.000000000000000000, 0.000000000000000000, 0.000000000000000000 ) ) ;
#10111 = AXIS2_PLACEMENT_3D ( 'NONE', #4876, #12181, #14 ) ;
#10112 = ORIENTED_EDGE ( 'NONE', *, *, #734, .F. ) ;
#10113 = EDGE_CURVE ( 'NONE', #9501, #645, #8232, .T. ) ;
#10114 = DIRECTION ( 'NONE',  ( 0.000000000000000000, 0.000000000000000000, 1.000000000000000000 ) ) ;
#10115 = ORIENTED_EDGE ( 'NONE', *, *, #9207, .T. ) ;
#10116 = CARTESIAN_POINT ( 'NONE',  ( 2.066987299999999639, 2.531329380823229670E-16, -0.7499999989075251117 ) ) ;
#10117 = CARTESIAN_POINT ( 'NONE',  ( -0.8737888311108684691, 5.936248257219528313, 18.50344185141215547 ) ) ;
#10118 = CIRCLE ( 'NONE', #1721, 1.499999999999999556 ) ;
#10119 = CARTESIAN_POINT ( 'NONE',  ( -0.4746045441281580013, 189.7004852670901585, 10.35781894787841573 ) ) ;
#10120 = DIRECTION ( 'NONE',  ( 0.000000000000000000, -1.000000000000000000, 0.000000000000000000 ) ) ;
#10121 = CARTESIAN_POINT ( 'NONE',  ( -1.530808498934191571E-16, 2.500000000000000000, 1.600000002184949865 ) ) ;
#10122 = CARTESIAN_POINT ( 'NONE',  ( -1.767766952966368432, -1.767766952966369320, -1.400000000000000133 ) ) ;
#10123 = AXIS2_PLACEMENT_3D ( 'NONE', #2464, #1344, #14643 ) ;
#10124 = DIRECTION ( 'NONE',  ( 0.000000000000000000, 0.000000000000000000, 1.000000000000000000 ) ) ;
#10125 = CARTESIAN_POINT ( 'NONE',  ( 2.500000000000000000, 3.061616997868383141E-16, -0.9999999978150501123 ) ) ;
#10126 = CARTESIAN_POINT ( 'NONE',  ( 3.796994071234844259E-16, -2.066987299999999639, -1.549999998907525045 ) ) ;
#10127 = EDGE_CURVE ( 'NONE', #11745, #3914, #8908, .T. ) ;
#10128 = CARTESIAN_POINT ( 'NONE',  ( 7.799024015210637373, -1.482594289697068746, 31.00000000000000000 ) ) ;
#10129 = DIRECTION ( 'NONE',  ( -1.000000000000000000, 0.000000000000000000, 0.000000000000000000 ) ) ;
#10130 = ORIENTED_EDGE ( 'NONE', *, *, #15184, .T. ) ;
#10131 = ORIENTED_EDGE ( 'NONE', *, *, #11259, .T. ) ;
#10132 = EDGE_CURVE ( 'NONE', #6522, #478, #13054, .T. ) ;
#10133 = ORIENTED_EDGE ( 'NONE', *, *, #160, .F. ) ;
#10134 = CARTESIAN_POINT ( 'NONE',  ( 5.747343991580196487, -1.727858744772237332, 30.00007997643738022 ) ) ;
#10135 = CARTESIAN_POINT ( 'NONE',  ( 3.882809187878947021, 4.899079348630040798, 4.025999019766705267 ) ) ;
#10136 = VERTEX_POINT ( 'NONE', #14091 ) ;
#10137 = CARTESIAN_POINT ( 'NONE',  ( -0.1306171417088603792, -6.000000000000000000, 4.000000000000004441 ) ) ;
#10138 = CARTESIAN_POINT ( 'NONE',  ( 0.1323736289505711150, -6.249999999999999112, 18.99999999999998934 ) ) ;
#10139 = CARTESIAN_POINT ( 'NONE',  ( 1.354942165116848791E-13, 6.250000000000000888, 16.99999999999998579 ) ) ;
#10140 = CARTESIAN_POINT ( 'NONE',  ( 2.500000000000000000, 3.061616997868383141E-16, -1.900000000000000133 ) ) ;
#10141 = CARTESIAN_POINT ( 'NONE',  ( -2.500000000000000444, 185.8999999978150584, 7.000000000000000000 ) ) ;
#10142 = CARTESIAN_POINT ( 'NONE',  ( 5.935543223013871383, -0.8771126767605965657, 11.63064961348853465 ) ) ;
#10143 = DIRECTION ( 'NONE',  ( 0.000000000000000000, 0.000000000000000000, 1.000000000000000000 ) ) ;
#10144 = DIRECTION ( 'NONE',  ( 0.000000000000000000, 1.000000000000000000, 0.000000000000000000 ) ) ;
#10145 = VECTOR ( 'NONE', #13837, 1000.000000000000000 ) ;
#10146 = CARTESIAN_POINT ( 'NONE',  ( -6.911788849595090767E-16, 187.7699999975965568, 9.500000000000001776 ) ) ;
#10147 = CARTESIAN_POINT ( 'NONE',  ( 0.8239120926223584274, 228.2181226988968774, 10.05946334177977519 ) ) ;
#10148 = CARTESIAN_POINT ( 'NONE',  ( -2.733336431741188566, 227.6877042401139022, 8.499448515046434949 ) ) ;
#10149 = ORIENTED_EDGE ( 'NONE', *, *, #11511, .F. ) ;
#10150 = CARTESIAN_POINT ( 'NONE',  ( -0.6060429735925918493, 188.9999999999195950, 9.429439317718889768 ) ) ;
#10151 = ORIENTED_EDGE ( 'NONE', *, *, #6320, .T. ) ;
#10152 = CARTESIAN_POINT ( 'NONE',  ( -5.935543223013850955, 0.8771126767607326791, 11.63236078583908650 ) ) ;
#10153 = CARTESIAN_POINT ( 'NONE',  ( 2.930922878467525194, -5.520395124723545877, 10.99610786875028445 ) ) ;
#10154 = AXIS2_PLACEMENT_3D ( 'NONE', #1997, #7974, #4158 ) ;
#10155 = CARTESIAN_POINT ( 'NONE',  ( -0.2622538972264160106, 6.245673238944475791, 5.973859943692001906 ) ) ;
#10156 = DIRECTION ( 'NONE',  ( 0.000000000000000000, 1.000000000000000000, 0.000000000000000000 ) ) ;
#10157 = CARTESIAN_POINT ( 'NONE',  ( 2.998004403696063580, 227.2514993113943547, 7.215655842644150830 ) ) ;
#10158 = CARTESIAN_POINT ( 'NONE',  ( -4.070863287254081087, -4.743975846881804515, 31.87305891554300530 ) ) ;
#10159 = CARTESIAN_POINT ( 'NONE',  ( -2.500000000000000000, 0.000000000000000000, 2.500000000000000000 ) ) ;
#10160 = DIRECTION ( 'NONE',  ( 0.000000000000000000, 0.000000000000000000, 1.000000000000000000 ) ) ;
#10161 = CARTESIAN_POINT ( 'NONE',  ( -4.435347140101025154, -4.403429997944519947, 30.86936067245787996 ) ) ;
#10162 = CARTESIAN_POINT ( 'NONE',  ( -1.767766952966369542, 185.2999999999999829, 8.767766952966368876 ) ) ;
#10163 = CARTESIAN_POINT ( 'NONE',  ( -1.814481855529834764, 227.9916279875985765, 6.215212007442850961 ) ) ;
#10164 = CARTESIAN_POINT ( 'NONE',  ( -2.066987299999999639, 0.000000000000000000, -2.549999998907525711 ) ) ;
#10165 = CARTESIAN_POINT ( 'NONE',  ( 4.344313232727052387, 4.493553492990165488, 12.00436969680152721 ) ) ;
#10166 = CARTESIAN_POINT ( 'NONE',  ( -0.8561741729129455081, 2.066987299999999639, 1.100000001092475088 ) ) ;
#10167 = CARTESIAN_POINT ( 'NONE',  ( 1.767766952966369320, 184.9000000000000057, 5.232233047033630235 ) ) ;
#10168 = CARTESIAN_POINT ( 'NONE',  ( 5.725930890718373689, -2.506952462183944075, 18.79933148907576523 ) ) ;
#10170 = ORIENTED_EDGE ( 'NONE', *, *, #13518, .T. ) ;
#10169 = CARTESIAN_POINT ( 'NONE',  ( -2.066987300000000527, 187.9999999989075263, 6.143825827087054492 ) ) ;
#10171 = EDGE_CURVE ( 'NONE', #12272, #12347, #10263, .T. ) ;
#10172 = CARTESIAN_POINT ( 'NONE',  ( 2.897581130414634077E-17, -9.750000000000003553, 2.000000000000001776 ) ) ;
#10173 = AXIS2_PLACEMENT_3D ( 'NONE', #2662, #10857, #6097 ) ;
#10174 = CARTESIAN_POINT ( 'NONE',  ( -5.000000000000000000, 0.000000000000000000, 5.000000000000004441 ) ) ;
#10175 =( BOUNDED_CURVE ( )  B_SPLINE_CURVE ( 2, ( #9935, #14787, #11200, #13578, #9065, #3003, #845, #6908, #4508 ),
 .UNSPECIFIED., .F., .F. ) 
 B_SPLINE_CURVE_WITH_KNOTS ( ( 3, 2, 2, 2, 3 ),
 ( 0.4285714285714285476, 0.4464285714285714524, 0.4642857142857143016, 0.4821428571428571508, 0.5000000000000000000 ),
 .UNSPECIFIED. ) 
 CURVE ( )  GEOMETRIC_REPRESENTATION_ITEM ( )  RATIONAL_B_SPLINE_CURVE ( ( 1.000000000000000000, 0.9238795325112867385, 1.000000000000000000, 0.9238795325112867385, 1.000000000000000000, 0.9238795325112867385, 1.000000000000000000, 0.9238795325112867385, 1.000000000000000000 ) ) 
 REPRESENTATION_ITEM ( '' )  );
#10176 = CARTESIAN_POINT ( 'NONE',  ( -5.531623157106191790, 2.327208526676369349, 4.126352953155773662 ) ) ;
#10177 = CARTESIAN_POINT ( 'NONE',  ( 2.435767896792930376, 189.0000000021955202, 7.586867367984001298 ) ) ;
#10178 = CARTESIAN_POINT ( 'NONE',  ( 0.001687421788282983956, -0.3999999999999906408, -2.472702538403935169 ) ) ;
#10179 = CARTESIAN_POINT ( 'NONE',  ( -2.913793338554793166E-15, 228.9118723800512782, 8.872930300147347182 ) ) ;
#10180 = CARTESIAN_POINT ( 'NONE',  ( 6.172651332693093629, -0.9815532474593722245, 5.261902130840119263 ) ) ;
#10181 = CARTESIAN_POINT ( 'NONE',  ( -5.558508435838135142, 2.857531096719037489, 24.49999999999999289 ) ) ;
#10182 = CARTESIAN_POINT ( 'NONE',  ( -5.931734679891438766, -0.9039278060244803070, 11.23617396794405288 ) ) ;
#10183 = VERTEX_POINT ( 'NONE', #10677 ) ;
#10184 = CARTESIAN_POINT ( 'NONE',  ( -2.066987300000000083, 186.4499999989075150, 7.000000000000000000 ) ) ;
#10185 = EDGE_LOOP ( 'NONE', ( #12095, #14166, #1293, #1700 ) ) ;
#10186 = CARTESIAN_POINT ( 'NONE',  ( -5.935543223013832304, 0.8771126767608681263, 24.63236078583910071 ) ) ;
#10187 = ADVANCED_FACE ( 'NONE', ( #3201 ), #5521, .F. ) ;
#10188 = ORIENTED_EDGE ( 'NONE', *, *, #14060, .T. ) ;
#10189 = CARTESIAN_POINT ( 'NONE',  ( -5.131373506000715068, 7.062729720844030723, 5.000000000000004441 ) ) ;
#10190 = EDGE_CURVE ( 'NONE', #12333, #8841, #15378, .T. ) ;
#10191 = CARTESIAN_POINT ( 'NONE',  ( 5.558508435838229289, -2.857531096718853192, 5.000000000000004441 ) ) ;
#10192 = ORIENTED_EDGE ( 'NONE', *, *, #7851, .F. ) ;
#10193 = B_SPLINE_CURVE_WITH_KNOTS ( 'NONE', 3,
 ( #3104, #12873, #7146, #3029, #8338, #2276, #8037, #5349, #12797, #15122, #4138, #14069, #6773, #7881, #13840, #3178, #2950, #12722 ),
 .UNSPECIFIED., .F., .F.,
 ( 4, 2, 2, 2, 2, 2, 2, 2, 4 ),
 ( 0.003131918686235972155, 0.003523310662250261557, 0.003914702638264551393, 0.004306094614278841229, 0.004697486590293131065, 0.005088878566307420900, 0.005480270542321711603, 0.005871662518336002307, 0.006263054494350292142 ),
 .UNSPECIFIED. ) ;
#10194 = CARTESIAN_POINT ( 'NONE',  ( -5.317509234263920526, -2.779225709351067053, 31.00000000000000000 ) ) ;
#10195 = EDGE_CURVE ( 'NONE', #5182, #10771, #14307, .T. ) ;
#10196 = CARTESIAN_POINT ( 'NONE',  ( 1.035533905932737531, 2.500000000000000444, -1.750000000000000222 ) ) ;
#10197 = CYLINDRICAL_SURFACE ( 'NONE', #8458, 1.499999999999999556 ) ;
#10198 = CARTESIAN_POINT ( 'NONE',  ( 1.767766952966369320, -1.767766952966368654, -1.200000000000000178 ) ) ;
#10199 = CARTESIAN_POINT ( 'NONE',  ( -5.648559266344516772, -2.676764518775952784, 5.613961794080713830 ) ) ;
#10200 = CARTESIAN_POINT ( 'NONE',  ( -2.782769401326322001, 5.315896561274772836, 17.49571079637979309 ) ) ;
#10201 = ITEM_DEFINED_TRANSFORMATION ( 'NONE', 'NONE', #4512,  #14201 ) ;
#10202 = CARTESIAN_POINT ( 'NONE',  ( 2.082642335314403343E-14, -6.250000000000000888, 31.00000000000000000 ) ) ;
#10203 = CARTESIAN_POINT ( 'NONE',  ( -0.8561741729129458411, -2.066987299999999195, 1.092474635061568626E-09 ) ) ;
#10204 = CARTESIAN_POINT ( 'NONE',  ( -0.2619041840694728007, 6.245686665308502583, 30.02605849433794916 ) ) ;
#10205 = ORIENTED_EDGE ( 'NONE', *, *, #4255, .F. ) ;
#10206 = EDGE_LOOP ( 'NONE', ( #14009, #13520, #1256, #1058 ) ) ;
#10207 = ORIENTED_EDGE ( 'NONE', *, *, #13868, .F. ) ;
#10208 = CARTESIAN_POINT ( 'NONE',  ( 4.069800786343747312, -4.744882212776869501, 18.87381964045070859 ) ) ;
#10209 = CARTESIAN_POINT ( 'NONE',  ( 6.020822430078776044, 1.681351817312468633, 4.025914576658297328 ) ) ;
#10210 = ORIENTED_EDGE ( 'NONE', *, *, #11796, .T. ) ;
#10211 = CARTESIAN_POINT ( 'NONE',  ( 5.746619684944318962, -1.730157667110693298, 19.00004932073311181 ) ) ;
#10212 = ADVANCED_FACE ( 'NONE', ( #3125 ), #6951, .F. ) ;
#10213 = CARTESIAN_POINT ( 'NONE',  ( 0.8736772044961308437, -6.188841968496043400, 17.49611573292809652 ) ) ;
#10214 = CARTESIAN_POINT ( 'NONE',  ( -0.8738043859789770273, 6.188821459035891870, 18.50341560223740700 ) ) ;
#10215 = CARTESIAN_POINT ( 'NONE',  ( 0.000000000000000000, 0.000000000000000000, 52.97056274847714263 ) ) ;
#10216 = CARTESIAN_POINT ( 'NONE',  ( -5.387129544537350156E-16, 185.2999999978150356, 9.500000000000001776 ) ) ;
#10217 = CARTESIAN_POINT ( 'NONE',  ( -1.767766952966369098, 1.767766952966369098, 2.406999999978150395 ) ) ;
#10218 = DIRECTION ( 'NONE',  ( 0.000000000000000000, -1.000000000000000000, 0.000000000000000000 ) ) ;
#10219 = CARTESIAN_POINT ( 'NONE',  ( 0.000000000000000000, 144.0000000000000000, 0.000000000000000000 ) ) ;
#10220 = EDGE_CURVE ( 'NONE', #4806, #15370, #10978, .T. ) ;
#10221 = AXIS2_PLACEMENT_3D ( 'NONE', #14598, #3610, #13241 ) ;
#10222 = CARTESIAN_POINT ( 'NONE',  ( 2.500000000000000444, 185.5699999975965397, 7.000000000000000000 ) ) ;
#10223 = CARTESIAN_POINT ( 'NONE',  ( -0.9967757174687167376, 228.8247258804818216, 8.621246238880397428 ) ) ;
#10224 = CARTESIAN_POINT ( 'NONE',  ( -0.7768053109583262783, 226.3575155338836282, 4.581995736916623763 ) ) ;
#10225 = VERTEX_POINT ( 'NONE', #6286 ) ;
#10226 = CARTESIAN_POINT ( 'NONE',  ( -1.698715844156870602, 1.839699740483268675, -2.499564404588821898 ) ) ;
#10227 = ORIENTED_EDGE ( 'NONE', *, *, #1127, .T. ) ;
#10228 = CARTESIAN_POINT ( 'NONE',  ( 3.253823204785213807, -5.337590213880445411, 5.873058915543009739 ) ) ;
#10229 = CARTESIAN_POINT ( 'NONE',  ( -6.021167129161029585, 1.680051667990390074, 23.52640428276697904 ) ) ;
#10230 = CARTESIAN_POINT ( 'NONE',  ( 0.5043776560898024508, -6.230795654995834987, 12.37337476296010230 ) ) ;
#10231 = CARTESIAN_POINT ( 'NONE',  ( 0.8738118504727695468, 5.936246475285000379, 25.00357242174242245 ) ) ;
#10232 = EDGE_CURVE ( 'NONE', #7970, #3737, #13354, .T. ) ;
#10233 = VECTOR ( 'NONE', #9389, 1000.000000000000000 ) ;
#10234 = CARTESIAN_POINT ( 'NONE',  ( 0.1881727879509562662, 228.2551366909677597, 10.16828399086544721 ) ) ;
#10235 = CARTESIAN_POINT ( 'NONE',  ( 2.817313151351107159, 5.579000502529474659, 5.130639327542138695 ) ) ;
#10236 = CARTESIAN_POINT ( 'NONE',  ( 4.290381260516251238, -4.545736887716230967, 17.38482219624156855 ) ) ;
#10237 = CARTESIAN_POINT ( 'NONE',  ( 2.066987300000000083, -0.8561741729129449530, -1.399999998907525134 ) ) ;
#10238 = CARTESIAN_POINT ( 'NONE',  ( -3.923477796648506377, -4.541042560386491012, 31.87303779027052286 ) ) ;
#10239 = DIRECTION ( 'NONE',  ( 0.000000000000000000, 0.000000000000000000, 1.000000000000000000 ) ) ;
#10240 = CARTESIAN_POINT ( 'NONE',  ( 1.035533905932737753, 186.5499999999999829, 4.500000000000000888 ) ) ;
#10241 = CARTESIAN_POINT ( 'NONE',  ( 0.7033144145436343031, 227.6506181221223244, 5.230356066017792571 ) ) ;
#10242 = PRODUCT_DEFINITION_CONTEXT ( 'detailed design', #7502, 'design' ) ;
#10243 = FACE_BOUND ( 'NONE', #12506, .T. ) ;
#10244 = VECTOR ( 'NONE', #4903, 1000.000000000000000 ) ;
#10245 = CARTESIAN_POINT ( 'NONE',  ( 5.903596343266361401, -2.055998103990403170, 25.49995078984292718 ) ) ;
#10246 = CARTESIAN_POINT ( 'NONE',  ( 0.8561741729129465073, -2.066987299999999195, -2.499999998907525445 ) ) ;
#10247 = CARTESIAN_POINT ( 'NONE',  ( -0.8561741729129458411, 188.4999999989074979, 4.933012699999999029 ) ) ;
#10248 = CARTESIAN_POINT ( 'NONE',  ( -5.783239563508375092, -1.602707436861291246, 18.97358595436693207 ) ) ;
#10250 = ORIENTED_EDGE ( 'NONE', *, *, #9912, .F. ) ;
#10249 = CARTESIAN_POINT ( 'NONE',  ( -1.461580736456473462, 186.5499999989075093, 8.461580736456472351 ) ) ;
#10251 = CARTESIAN_POINT ( 'NONE',  ( -4.416837305303536354, -4.422286678978971430, 17.73809786915987630 ) ) ;
#10252 = CARTESIAN_POINT ( 'NONE',  ( 5.915755444410828012, -1.003187219519705353, 17.49687951097622474 ) ) ;
#10253 = CARTESIAN_POINT ( 'NONE',  ( -5.999999999999999112, 201.6409668649147022, 13.30942870683726120 ) ) ;
#10254 = CARTESIAN_POINT ( 'NONE',  ( 5.000000000000000000, 6.123233995736766282E-16, 5.000000000000004441 ) ) ;
#10255 = CARTESIAN_POINT ( 'NONE',  ( 2.572874078457004998, 189.3734677023459199, 5.473824851193815455 ) ) ;
#10256 = CARTESIAN_POINT ( 'NONE',  ( -5.131373506000715068, 7.062729720844030723, 5.000000000000004441 ) ) ;
#10257 = CARTESIAN_POINT ( 'NONE',  ( -1.265664690411614835E-16, 2.066987299999999639, -2.949999998907525178 ) ) ;
#10258 = CARTESIAN_POINT ( 'NONE',  ( 0.9770418472818584998, 189.7111507403969881, 10.22957020356571967 ) ) ;
#10259 = CARTESIAN_POINT ( 'NONE',  ( -4.142620314836367612, 4.341347824677513678, 30.38557478428061032 ) ) ;
#10260 = DIRECTION ( 'NONE',  ( 0.000000000000000000, 1.000000000000000000, 0.000000000000000000 ) ) ;
#10261 = ORIENTED_EDGE ( 'NONE', *, *, #11959, .T. ) ;
#10262 = CARTESIAN_POINT ( 'NONE',  ( -2.066987300000000971, 186.4999999989075263, 7.856174172912944620 ) ) ;
#10263 = CIRCLE ( 'NONE', #12286, 12.50000000000000533 ) ;
#10264 = ORIENTED_EDGE ( 'NONE', *, *, #15541, .T. ) ;
#10265 = CARTESIAN_POINT ( 'NONE',  ( -5.486741141153698820, -2.429871531109943028, 23.70111757752058068 ) ) ;
#10266 =( REPRESENTATION_RELATIONSHIP ('NONE','NONE', #11191, #3660 ) REPRESENTATION_RELATIONSHIP_WITH_TRANSFORMATION ( #15699 )SHAPE_REPRESENTATION_RELATIONSHIP( ) );
#10267 = ORIENTED_EDGE ( 'NONE', *, *, #10776, .T. ) ;
#10268 = DIRECTION ( 'NONE',  ( 0.000000000000000000, -1.000000000000000000, 0.000000000000000000 ) ) ;
#10269 = FILL_AREA_STYLE ('',( #1589 ) ) ;
#10270 = CARTESIAN_POINT ( 'NONE',  ( -5.746996058422763731, -1.729015645941962775, 29.99992038825523721 ) ) ;
#10271 = CARTESIAN_POINT ( 'NONE',  ( -0.2619456584320733472, 5.995505046955622142, 17.02607193928647078 ) ) ;
#10272 = CARTESIAN_POINT ( 'NONE',  ( 5.317509234264066187, -2.779225709350791274, 24.36763921416088863 ) ) ;
#10273 = CARTESIAN_POINT ( 'NONE',  ( 2.500000000000000444, 1.035533905932737975, -1.050000000000000044 ) ) ;
#10274 = CARTESIAN_POINT ( 'NONE',  ( 1.767766952966368654, 1.767766952966369098, 2.200000000000000178 ) ) ;
#10275 = CARTESIAN_POINT ( 'NONE',  ( -3.107688324358672372, -5.133887830459857859, 10.62621569129737331 ) ) ;
#10276 = ADVANCED_FACE ( 'NONE', ( #13201, #14552 ), #9714, .T. ) ;
#10277 = CARTESIAN_POINT ( 'NONE',  ( -5.558508435838095174, -2.857531096719115649, 24.49999999999999289 ) ) ;
#10278 = CARTESIAN_POINT ( 'NONE',  ( 2.066987299999999639, 0.8561741729129456191, -1.299999998907525267 ) ) ;
#10279 = CARTESIAN_POINT ( 'NONE',  ( 4.286401442266483564, 4.198423832313243231, 11.49999999999998224 ) ) ;
#10280 = EDGE_CURVE ( 'NONE', #1532, #1004, #5970, .T. ) ;
#10281 = ORIENTED_EDGE ( 'NONE', *, *, #13291, .T. ) ;
#10282 = VERTEX_POINT ( 'NONE', #1260 ) ;
#10283 = EDGE_CURVE ( 'NONE', #7176, #4447, #12003, .T. ) ;
#10284 = VERTEX_POINT ( 'NONE', #9942 ) ;
#10285 = CARTESIAN_POINT ( 'NONE',  ( 3.458623254138677883, -5.207221900902841760, 18.97377282875267568 ) ) ;
#10286 = CARTESIAN_POINT ( 'NONE',  ( 3.659182332138577465E-16, 195.9933836657089898, 6.233275261299416670 ) ) ;
#10287 = ORIENTED_EDGE ( 'NONE', *, *, #15038, .F. ) ;
#10288 = CARTESIAN_POINT ( 'NONE',  ( 5.317509234264033324, -2.779225709350852114, 17.99999999999998934 ) ) ;
#10289 = CARTESIAN_POINT ( 'NONE',  ( -1.530808498934191571E-16, 2.500000000000000000, -0.7999999978150507118 ) ) ;
#10290 = AXIS2_PLACEMENT_3D ( 'NONE', #4388, #6705, #4146 ) ;
#10291 = CARTESIAN_POINT ( 'NONE',  ( -5.866923913994661177, 1.260079467906454198, 5.799520541027148646 ) ) ;
#10292 = CYLINDRICAL_SURFACE ( 'NONE', #11267, 6.000000000000000000 ) ;
#10293 = CARTESIAN_POINT ( 'NONE',  ( 2.500000000000000000, 188.6999999978150697, 7.000000000000000000 ) ) ;
#10295 = CARTESIAN_POINT ( 'NONE',  ( -5.385276659965230388E-16, 226.3251816629291966, 4.486670979098442480 ) ) ;
#10294 = B_SPLINE_CURVE_WITH_KNOTS ( 'NONE', 3,
 ( #9417, #4485, #10377, #10686, #11792, #820, #10607, #9188, #15546, #6728, #7035, #12909, #12827, #13947, #657, #11865, #8149, #3056 ),
 .UNSPECIFIED., .F., .F.,
 ( 4, 2, 2, 2, 2, 2, 2, 2, 4 ),
 ( 0.000000000000000000, 0.0003914357524127495998, 0.0007828715048254991996, 0.001174307257238248799, 0.001565743009650997315, 0.001957178762063746264, 0.002348614514476494563, 0.002740050266889243295, 0.003131486019301992028 ),
 .UNSPECIFIED. ) ;
#10296 = CARTESIAN_POINT ( 'NONE',  ( 4.267558728637154353, 4.217879122113844303, 11.23617396794405465 ) ) ;
#10297 = EDGE_CURVE ( 'NONE', #11831, #11875, #8525, .T. ) ;
#10298 = DIRECTION ( 'NONE',  ( 1.000000000000000000, 0.000000000000000000, 1.047444401652940007E-14 ) ) ;
#10299 = CARTESIAN_POINT ( 'NONE',  ( -2.500000000000000444, 188.3199999975965682, 5.964466094067261359 ) ) ;
#10300 = CARTESIAN_POINT ( 'NONE',  ( 2.438651006298347301, 227.8520175407923034, 8.982830694042164055 ) ) ;
#10301 = CARTESIAN_POINT ( 'NONE',  ( -0.9181233697252281223, 226.3712865412501003, 4.622592831843514993 ) ) ;
#10302 = ORIENTED_EDGE ( 'NONE', *, *, #2694, .F. ) ;
#10303 = CARTESIAN_POINT ( 'NONE',  ( -1.983218494070152493, 1.528667308324898944, -2.500812883383392915 ) ) ;
#10304 = ORIENTED_EDGE ( 'NONE', *, *, #7177, .F. ) ;
#10305 = CARTESIAN_POINT ( 'NONE',  ( -0.6151877315909501931, 6.220340188096019851, 12.29906673469665712 ) ) ;
#10306 = ADVANCED_BREP_SHAPE_REPRESENTATION ( '', ( #4889, #14201 ), #2994 ) ;
#10307 = CARTESIAN_POINT ( 'NONE',  ( -9.750000000000003553, 19.99999999999999645, -3.401296724241641415E-14 ) ) ;
#10308 = CARTESIAN_POINT ( 'NONE',  ( 0.000000000000000000, 0.000000000000000000, 2.500000000000000000 ) ) ;
#10309 = DIRECTION ( 'NONE',  ( 0.000000000000000000, 0.000000000000000000, -1.000000000000000000 ) ) ;
#10310 = CARTESIAN_POINT ( 'NONE',  ( 4.286401442266448036, -4.198423832313277870, 24.49999999999999289 ) ) ;
#10311 = CARTESIAN_POINT ( 'NONE',  ( -1.035533905932738197, -2.500000000000000000, 1.850000000000000311 ) ) ;
#10312 = CARTESIAN_POINT ( 'NONE',  ( -2.500000000000000444, 1.035533905932737753, -0.7500000000000004441 ) ) ;
#10313 = FILL_AREA_STYLE ('',( #5234 ) ) ;
#10314 = CARTESIAN_POINT ( 'NONE',  ( -2.817313151351126255, -5.579000502529464001, 31.00000000000000000 ) ) ;
#10315 = CARTESIAN_POINT ( 'NONE',  ( -2.500000000000000444, 185.0499999978150640, 5.964466094067261359 ) ) ;
#10316 = CARTESIAN_POINT ( 'NONE',  ( 0.06504883222449296676, 227.6089665442046339, 5.110063933342379627 ) ) ;
#10317 = FACE_BOUND ( 'NONE', #12175, .T. ) ;
#10318 = ADVANCED_FACE ( 'NONE', ( #11049 ), #1609, .T. ) ;
#10319 = CARTESIAN_POINT ( 'NONE',  ( -5.330004929009555248, 2.755647751839462423, 18.26239891805597537 ) ) ;
#10320 = CARTESIAN_POINT ( 'NONE',  ( 1.461580736456473018, -1.461580736456472573, -1.649999998907525356 ) ) ;
#10321 = PRODUCT_DEFINITION ( 'UNKNOWN', '', #13643, #4189 ) ;
#10322 = CARTESIAN_POINT ( 'NONE',  ( -2.500000000000000444, 186.0000000000000000, 7.000000000000000000 ) ) ;
#10323 = LINE ( 'NONE', #9139, #5312 ) ;
#10324 = ADVANCED_FACE ( 'NONE', ( #2377 ), #15675, .F. ) ;
#10326 = VERTEX_POINT ( 'NONE', #6136 ) ;
#10325 = CARTESIAN_POINT ( 'NONE',  ( 2.066987299999999639, 187.5999999989075491, 7.856174172912946396 ) ) ;
#10327 = CARTESIAN_POINT ( 'NONE',  ( -4.143041610105390404, -4.340967609746952505, 17.38602261056918152 ) ) ;
#10328 = FACE_OUTER_BOUND ( 'NONE', #318, .T. ) ;
#10329 = CARTESIAN_POINT ( 'NONE',  ( -5.317509234263873452, 2.779225709351155871, 24.36935038651144581 ) ) ;
#10330 =( NAMED_UNIT ( * ) PLANE_ANGLE_UNIT ( ) SI_UNIT ( $, .RADIAN. ) );
#10331 = CARTESIAN_POINT ( 'NONE',  ( 2.082142646712863421, 190.0100437745609554, 5.053690205712503491 ) ) ;
#10332 = CARTESIAN_POINT ( 'NONE',  ( 2.500000000000000444, 187.8999999978150584, 7.000000000000000000 ) ) ;
#10333 = DIRECTION ( 'NONE',  ( -0.000000000000000000, -1.000000000000000000, -0.000000000000000000 ) ) ;
#10334 = CARTESIAN_POINT ( 'NONE',  ( 1.986575337946455022, 228.3035988107396292, 7.116201538324070874 ) ) ;
#10335 = CARTESIAN_POINT ( 'NONE',  ( 5.859155363331463917, -2.178872204144761682, 23.52599901976669727 ) ) ;
#10336 = CARTESIAN_POINT ( 'NONE',  ( 5.558508435838199979, 2.857531096718914476, 31.00000000000000000 ) ) ;
#10337 = DIRECTION ( 'NONE',  ( 0.000000000000000000, 1.000000000000000000, 0.000000000000000000 ) ) ;
#10338 = ORIENTED_EDGE ( 'NONE', *, *, #9439, .T. ) ;
#10339 = CARTESIAN_POINT ( 'NONE',  ( -1.461580736456473462, 188.9499999989075150, 8.461580736456472351 ) ) ;
#10340 = CARTESIAN_POINT ( 'NONE',  ( -0.6139908388540374906, 5.969238533166618232, 10.69977627912011364 ) ) ;
#10341 = ORIENTED_EDGE ( 'NONE', *, *, #2616, .T. ) ;
#10342 = DIRECTION ( 'NONE',  ( -0.000000000000000000, 1.000000000000000000, -0.000000000000000000 ) ) ;
#10343 = CARTESIAN_POINT ( 'NONE',  ( 4.404571325722361763E-17, 185.7999999999999829, 4.500000000000000000 ) ) ;
#10344 = DIRECTION ( 'NONE',  ( 1.251928832280965695E-16, 1.000000000000000000, 0.000000000000000000 ) ) ;
#10345 = MANIFOLD_SOLID_BREP ( 'Extrude-Thin1', #14349 ) ;
#10346 = CARTESIAN_POINT ( 'NONE',  ( -3.567258970015968256, 5.133675764669679786, 3.999917806784441865 ) ) ;
#10347 = DIRECTION ( 'NONE',  ( -0.000000000000000000, 1.000000000000000000, -0.000000000000000000 ) ) ;
#10348 = CARTESIAN_POINT ( 'NONE',  ( 5.531757352715673370, -2.326874507723157848, 23.62619317285289000 ) ) ;
#10349 = CARTESIAN_POINT ( 'NONE',  ( -1.035533905932737753, 2.500000000000000444, 1.650000002184949910 ) ) ;
#10350 = CARTESIAN_POINT ( 'NONE',  ( 4.592425496802573972E-16, -2.500000000000000000, -1.300000000000000044 ) ) ;
#10351 = CARTESIAN_POINT ( 'NONE',  ( -5.999999999999999112, 187.9952603975225429, 3.440894205938198613 ) ) ;
#10352 = CARTESIAN_POINT ( 'NONE',  ( 2.500000000000000444, 187.0999999978150754, 7.000000000000000000 ) ) ;
#10353 = CARTESIAN_POINT ( 'NONE',  ( -1.084202172485504434E-16, 3.464101615137754830, -5.500000000000000000 ) ) ;
#10354 = CARTESIAN_POINT ( 'NONE',  ( 3.459597053047831494, 5.206576120509754269, 31.97408542334170178 ) ) ;
#10355 = CARTESIAN_POINT ( 'NONE',  ( -0.5043776560897315075, 6.230795654995839428, 31.87337476296010053 ) ) ;
#10356 = CONICAL_SURFACE ( 'NONE', #10613, 2.575022672948154234, 0.08726646259971664044 ) ;
#10357 = VERTEX_POINT ( 'NONE', #13438 ) ;
#10358 = ORIENTED_EDGE ( 'NONE', *, *, #12029, .F. ) ;
#10359 = ORIENTED_EDGE ( 'NONE', *, *, #586, .T. ) ;
#10360 = CARTESIAN_POINT ( 'NONE',  ( 4.435347140100977192, -4.403429997944567020, 17.99999999999998934 ) ) ;
#10361 = DIRECTION ( 'NONE',  ( 0.000000000000000000, 0.000000000000000000, 1.000000000000000000 ) ) ;
#10362 = EDGE_LOOP ( 'NONE', ( #13346, #10264, #1758, #9803 ) ) ;
#10363 = VECTOR ( 'NONE', #12547, 1000.000000000000114 ) ;
#10364 =( NAMED_UNIT ( * ) SI_UNIT ( $, .STERADIAN. ) SOLID_ANGLE_UNIT ( ) );
#10365 = EDGE_CURVE ( 'NONE', #2495, #4594, #2636, .T. ) ;
#10366 = CARTESIAN_POINT ( 'NONE',  ( 2.500000000000000444, -1.035533905932737309, 0.5500000021849495990 ) ) ;
#10367 = CARTESIAN_POINT ( 'NONE',  ( -5.915641100987839351, 1.003868594704703021, 5.504289203620185589 ) ) ;
#10368 = CARTESIAN_POINT ( 'NONE',  ( -4.291255145203995980, -4.544933371694754420, 4.386038205919295940 ) ) ;
#10369 = CARTESIAN_POINT ( 'NONE',  ( 2.066987299999999639, 185.1999999989075150, 7.856174172912946396 ) ) ;
#10370 = CARTESIAN_POINT ( 'NONE',  ( 2.500000000000000000, 3.061616997868383141E-16, 2.106999999978150129 ) ) ;
#10371 = B_SPLINE_CURVE_WITH_KNOTS ( 'NONE', 3,
 ( #11816, #12775, #1879, #6835, #1006, #5868, #10716 ),
 .UNSPECIFIED., .F., .F.,
 ( 4, 3, 4 ),
 ( 0.004378233155234298977, 0.004805482862474828344, 0.005139916140553234432 ),
 .UNSPECIFIED. ) ;
#10372 = CARTESIAN_POINT ( 'NONE',  ( 5.915755444410811137, 1.003187219519795725, 18.50312048902376461 ) ) ;
#10373 = SHAPE_DEFINITION_REPRESENTATION ( #14518, #4596 ) ;
#10374 = CARTESIAN_POINT ( 'NONE',  ( 2.066987299999999639, 0.8561741729129456191, 1.700000001092474733 ) ) ;
#10375 = CARTESIAN_POINT ( 'NONE',  ( 2.500000000000000444, 188.0199999975965852, 5.964466094067262247 ) ) ;
#10376 = CARTESIAN_POINT ( 'NONE',  ( 2.467000123265670641, 227.8390626820829823, 8.944723654098295285 ) ) ;
#10377 = CARTESIAN_POINT ( 'NONE',  ( 4.416779112813551400, 4.422345839825900349, 18.26225281721714921 ) ) ;
#10378 = VECTOR ( 'NONE', #5286, 1000.000000000000000 ) ;
#10379 = ORIENTED_EDGE ( 'NONE', *, *, #457, .T. ) ;
#10380 = CARTESIAN_POINT ( 'NONE',  ( -2.515015366234329530, -0.07938793225241053131, -2.500633784899425560 ) ) ;
#10381 = VERTEX_POINT ( 'NONE', #12840 ) ;
#10382 = CARTESIAN_POINT ( 'NONE',  ( -0.5043776560897083039, 6.230795654995842980, 12.37337476296007743 ) ) ;
#10383 = ADVANCED_FACE ( 'NONE', ( #10466 ), #2021, .T. ) ;
#10384 = LINE ( 'NONE', #12989, #1229 ) ;
#10385 = CARTESIAN_POINT ( 'NONE',  ( 6.143143148203074055, 1.154591847827623141, 23.88603820591927729 ) ) ;
#10386 = EDGE_LOOP ( 'NONE', ( #1103, #8432 ) ) ;
#10387 = CARTESIAN_POINT ( 'NONE',  ( 4.344265632482074757, 4.493596842504970823, 10.99574050496990196 ) ) ;
#10388 = AXIS2_PLACEMENT_3D ( 'NONE', #10189, #8927, #13760 ) ;
#10389 = CARTESIAN_POINT ( 'NONE',  ( -0.2623718222033166181, -6.245654667075793753, 23.52627829713834728 ) ) ;
#10390 = AXIS2_PLACEMENT_3D ( 'NONE', #2870, #3026, #7718 ) ;
#10391 = CARTESIAN_POINT ( 'NONE',  ( 4.153663429050745037, -4.670992970568404345, 17.20066851092423121 ) ) ;
#10392 = B_SPLINE_CURVE_WITH_KNOTS ( 'NONE', 3,
 ( #10975, #5815, #13038, #13205, #3494, #8445, #8528, #7007, #14477, #13281, #15518, #14301, #74, #5892, #8365, #12166, #9717, #2298 ),
 .UNSPECIFIED., .F., .F.,
 ( 4, 2, 2, 2, 2, 2, 2, 2, 4 ),
 ( 0.003131918686235972155, 0.003523310662250263292, 0.003914702638264554863, 0.004306094614278846433, 0.004697486590293137136, 0.005088878566307428707, 0.005480270542321718542, 0.005871662518336009245, 0.006263054494350299081 ),
 .UNSPECIFIED. ) ;
#10393 = CARTESIAN_POINT ( 'NONE',  ( -2.500000000000000000, -1.035533905932739307, -1.450000000000000400 ) ) ;
#10394 = CARTESIAN_POINT ( 'NONE',  ( 2.500000000000000000, 188.7500000000000000, 8.035533905932739529 ) ) ;
#10395 = CARTESIAN_POINT ( 'NONE',  ( 0.01925117833309565596, 0.4000000000000027978, -2.511168856671952554 ) ) ;
#10396 = CARTESIAN_POINT ( 'NONE',  ( 1.767766952966368654, 186.1999999978150697, 8.767766952966368876 ) ) ;
#10397 = CARTESIAN_POINT ( 'NONE',  ( -1.361424426418679889, 228.7361946629245892, 8.365563033085530620 ) ) ;
#10398 = CARTESIAN_POINT ( 'NONE',  ( -2.668367453516752974, -5.373994336898072710, 17.99999999999998934 ) ) ;
#10399 = CARTESIAN_POINT ( 'NONE',  ( 0.2637975869348134772, 6.245592211692891027, 25.47332839949195460 ) ) ;
#10400 = CARTESIAN_POINT ( 'NONE',  ( 2.066987299999999639, 2.531329380823229670E-16, -0.7499999989075251117 ) ) ;
#10401 = CARTESIAN_POINT ( 'NONE',  ( -2.500000000000000444, 185.9500000000000455, 5.964466094067261359 ) ) ;
#10402 = DIRECTION ( 'NONE',  ( 0.000000000000000000, 1.000000000000000000, 0.000000000000000000 ) ) ;
#10404 = EDGE_LOOP ( 'NONE', ( #2392, #10828 ) ) ;
#10403 = CARTESIAN_POINT ( 'NONE',  ( -2.066760391300492827E-16, 189.4499999989075150, 4.933012699999999029 ) ) ;
#10405 = CYLINDRICAL_SURFACE ( 'NONE', #13991, 1.000000000000000666 ) ;
#10406 = EDGE_CURVE ( 'NONE', #15622, #4492, #2553, .T. ) ;
#10407 = CARTESIAN_POINT ( 'NONE',  ( 2.500000000000000444, 186.4000000000000057, 7.000000000000000000 ) ) ;
#10408 = CARTESIAN_POINT ( 'NONE',  ( -13.50000000000000000, -0.001000000000000132727, 2.479909768273400161E-15 ) ) ;
#10409 = CARTESIAN_POINT ( 'NONE',  ( 5.935543223013866942, 0.8771126767606117758, 17.99999999999998934 ) ) ;
#10410 = MECHANICAL_DESIGN_GEOMETRIC_PRESENTATION_REPRESENTATION (  '', ( #14459 ), #7602 ) ;
#10411 = CARTESIAN_POINT ( 'NONE',  ( 0.9656511489911946411, 189.0000000017439845, 4.686691485181459171 ) ) ;
#10412 = CARTESIAN_POINT ( 'NONE',  ( 2.668367453516524268, -5.373994336898184621, 24.49999999999999289 ) ) ;
#10413 = CARTESIAN_POINT ( 'NONE',  ( -5.746837578676003311, -1.729433780394259879, 5.999950536462232087 ) ) ;
#10414 = CARTESIAN_POINT ( 'NONE',  ( 1.989910900261709470, 228.2393533748197569, 6.930657055068108363 ) ) ;
#10415 = CARTESIAN_POINT ( 'NONE',  ( 5.903596343266293012, -2.055998103990597681, 5.999950789842938725 ) ) ;
#10416 = CARTESIAN_POINT ( 'NONE',  ( 0.006257361140793449295, 0.4000000000000027978, 2.486236325722958718 ) ) ;
#10417 = CARTESIAN_POINT ( 'NONE',  ( 2.500000000000000000, 3.061616997868383141E-16, 1.400000002184949910 ) ) ;
#10418 = ORIENTED_EDGE ( 'NONE', *, *, #5519, .T. ) ;
#10419 = CARTESIAN_POINT ( 'NONE',  ( 2.066987300000000083, 184.9999999989074979, 7.856174172912946396 ) ) ;
#10420 = CARTESIAN_POINT ( 'NONE',  ( 4.267558728637180998, 4.217879122113815882, 30.73617396794403689 ) ) ;
#10421 = ORIENTED_EDGE ( 'NONE', *, *, #15050, .T. ) ;
#10422 = AXIS2_PLACEMENT_3D ( 'NONE', #3954, #10093, #6523 ) ;
#10423 = CARTESIAN_POINT ( 'NONE',  ( 5.317509234264033324, -2.779225709350852114, 17.99999999999998934 ) ) ;
#10424 = CARTESIAN_POINT ( 'NONE',  ( -2.692215568229726852, -5.362327947133653794, 4.737709621640688873 ) ) ;
#10425 = CARTESIAN_POINT ( 'NONE',  ( -7.180990026460726483, -3.384707322287581199, 11.49999999999998224 ) ) ;
#10426 = CARTESIAN_POINT ( 'NONE',  ( 1.461580736456473018, 184.5499999989075093, 5.538419263543527649 ) ) ;
#10427 = CARTESIAN_POINT ( 'NONE',  ( 4.435347140100914132, 4.403429997944631857, 17.99999999999998934 ) ) ;
#10428 = CARTESIAN_POINT ( 'NONE',  ( -13.50000000000000000, -0.001000000000000132727, 2.000000000000002220 ) ) ;
#10429 = EDGE_CURVE ( 'NONE', #642, #3364, #2438, .T. ) ;
#10430 = CARTESIAN_POINT ( 'NONE',  ( -4.154121946520847430, -4.670585111242995247, 5.798878384233395522 ) ) ;
#10431 = CARTESIAN_POINT ( 'NONE',  ( 2.500000000000000444, -1.035533905932737309, -1.949999999999999956 ) ) ;
#10432 = CARTESIAN_POINT ( 'NONE',  ( -5.725684683139609099, -2.507514573674767266, 4.201121615766616024 ) ) ;
#10433 = CARTESIAN_POINT ( 'NONE',  ( 5.999999999999999112, 195.9172377311516016, 6.220370292208427188 ) ) ;
#10434 = DIRECTION ( 'NONE',  ( -0.3090169943749579429, 0.9510565162951502005, 0.000000000000000000 ) ) ;
#10435 = CARTESIAN_POINT ( 'NONE',  ( 4.286401442266437378, 4.198423832313292081, 17.99999999999998934 ) ) ;
#10436 = FACE_OUTER_BOUND ( 'NONE', #5824, .T. ) ;
#10437 = EDGE_LOOP ( 'NONE', ( #2967, #9649, #14811, #7580 ) ) ;
#10438 = ORIENTED_EDGE ( 'NONE', *, *, #12522, .T. ) ;
#10439 = ORIENTED_EDGE ( 'NONE', *, *, #993, .T. ) ;
#10440 = CARTESIAN_POINT ( 'NONE',  ( 4.290130679986521756, -4.545972905167772637, 18.61560192892921606 ) ) ;
#10441 = CARTESIAN_POINT ( 'NONE',  ( 6.123233995736766282E-16, -6.250000000000000888, 5.000000000000004441 ) ) ;
#10442 = ORIENTED_EDGE ( 'NONE', *, *, #4773, .T. ) ;
#10443 = SURFACE_SIDE_STYLE ('',( #11706 ) ) ;
#10444 = CARTESIAN_POINT ( 'NONE',  ( 2.500000000000000444, -1.035533905932737309, -0.2499999978150505286 ) ) ;
#10445 = CARTESIAN_POINT ( 'NONE',  ( 6.143020266950989239, 1.155160780047645552, 18.61441947245482709 ) ) ;
#10446 = CARTESIAN_POINT ( 'NONE',  ( -4.344502777243494762, -4.493369211529300244, 4.496107868750330638 ) ) ;
#10447 = CARTESIAN_POINT ( 'NONE',  ( -0.8561741729129455081, 185.4999999989075548, 4.933012699999999029 ) ) ;
#10448 = CARTESIAN_POINT ( 'NONE',  ( -1.035533905932737753, 2.500000000000000444, 1.556999999978150750 ) ) ;
#10449 = APPLICATION_CONTEXT ( 'automotive_design' ) ;
#10450 = DIRECTION ( 'NONE',  ( 0.000000000000000000, -1.000000000000000000, 0.000000000000000000 ) ) ;
#10451 = CONTEXT_DEPENDENT_SHAPE_REPRESENTATION ( #6697, #10990 ) ;
#10452 = CARTESIAN_POINT ( 'NONE',  ( -1.461580736456472351, -1.461580736456473018, 0.5500000010924748217 ) ) ;
#10453 = CARTESIAN_POINT ( 'NONE',  ( -5.915641100987822476, -1.003868594704795836, 4.495710796379801977 ) ) ;
#10454 = CARTESIAN_POINT ( 'NONE',  ( -1.058356156152139738, 226.3870070917984094, 4.668936284651906909 ) ) ;
#10455 = MANIFOLD_SOLID_BREP ( 'Thread1', #15128 ) ;
#10456 = FACE_OUTER_BOUND ( 'NONE', #3896, .T. ) ;
#10457 = ORIENTED_EDGE ( 'NONE', *, *, #12454, .F. ) ;
#10458 = CARTESIAN_POINT ( 'NONE',  ( 4.592425496802573972E-16, -2.500000000000000000, 0.4000000021849499099 ) ) ;
#10459 = ORIENTED_EDGE ( 'NONE', *, *, #10132, .F. ) ;
#10460 = CARTESIAN_POINT ( 'NONE',  ( -0.8002720181890271567, 6.199262377003415203, 10.88606262465555119 ) ) ;
#10461 = DIRECTION ( 'NONE',  ( -0.9510565162951545304, 0.3090169943749447867, 0.000000000000000000 ) ) ;
#10462 = CARTESIAN_POINT ( 'NONE',  ( -6.176542424588117974, 0.9554180641285661135, 31.00000000000000000 ) ) ;
#10463 = EDGE_LOOP ( 'NONE', ( #2811, #4465, #3197, #8482 ) ) ;
#10464 = CARTESIAN_POINT ( 'NONE',  ( -4.435347140101154828, -4.403429997944389385, 24.49999999999999289 ) ) ;
#10465 = CARTESIAN_POINT ( 'NONE',  ( 2.094888803305876858E-14, -6.250000000000000888, 30.00000000000000000 ) ) ;
#10466 = FACE_OUTER_BOUND ( 'NONE', #7299, .T. ) ;
#10467 = CARTESIAN_POINT ( 'NONE',  ( 4.592425496802573972E-16, -2.500000000000000000, -0.5000000000000000000 ) ) ;
#10468 = CARTESIAN_POINT ( 'NONE',  ( -7.490007020835642848, -2.433650805992559896, 24.49999999999999289 ) ) ;
#10469 = PRESENTATION_STYLE_ASSIGNMENT (( #8163 ) ) ;
#10470 = CARTESIAN_POINT ( 'NONE',  ( 0.000000000000000000, 0.000000000000000000, 36.00000000000000711 ) ) ;
#10471 = CARTESIAN_POINT ( 'NONE',  ( -1.767766952966369765, 187.7000000000000171, 8.767766952966368876 ) ) ;
#10472 = EDGE_CURVE ( 'NONE', #8099, #13328, #14013, .T. ) ;
#10473 = CARTESIAN_POINT ( 'NONE',  ( -1.312946155259101522, 228.7505583286450985, 8.407046118935697976 ) ) ;
#10474 = CARTESIAN_POINT ( 'NONE',  ( 6.143020266951007002, -1.155160780047555180, 17.38558052754515160 ) ) ;
#10475 = CARTESIAN_POINT ( 'NONE',  ( -5.931734679891438766, 0.9039278060244781976, 18.26382603205596311 ) ) ;
#10476 = EDGE_CURVE ( 'NONE', #13364, #2492, #14514, .T. ) ;
#10477 = CARTESIAN_POINT ( 'NONE',  ( 0.8561741729129452860, 2.066987299999999639, -0.5999999989075253115 ) ) ;
#10478 = CIRCLE ( 'NONE', #3612, 5.000000000000000000 ) ;
#10479 = CARTESIAN_POINT ( 'NONE',  ( -1.767766952966369765, 187.7000000000000171, 8.767766952966368876 ) ) ;
#10480 = CARTESIAN_POINT ( 'NONE',  ( 2.817313151351005462, -5.579000502529526173, 24.63060690723498070 ) ) ;
#10481 = EDGE_CURVE ( 'NONE', #10326, #8787, #7767, .T. ) ;
#10483 = EDGE_LOOP ( 'NONE', ( #67, #13332, #7426, #1778 ) ) ;
#10482 = LINE ( 'NONE', #15335, #12335 ) ;
#10484 = DIRECTION ( 'NONE',  ( 0.000000000000000000, 0.000000000000000000, 1.000000000000000000 ) ) ;
#10485 = ORIENTED_EDGE ( 'NONE', *, *, #10028, .T. ) ;
#10486 = CARTESIAN_POINT ( 'NONE',  ( -5.000000000000000000, 0.000000000000000000, 36.00000000000000711 ) ) ;
#10487 = CARTESIAN_POINT ( 'NONE',  ( -2.433389886697037152, 189.7888483223419200, 9.123136959575992577 ) ) ;
#10488 = AXIS2_PLACEMENT_3D ( 'NONE', #6722, #2974, #11556 ) ;
#10489 = CARTESIAN_POINT ( 'NONE',  ( 1.767766952966369320, -1.767766952966368654, -0.2999999978150504343 ) ) ;
#10490 = CARTESIAN_POINT ( 'NONE',  ( -5.131373506000823426, 7.062729720843950787, 17.99999999999998934 ) ) ;
#10491 = CARTESIAN_POINT ( 'NONE',  ( -0.9735856429312665927, 5.920699391845031023, 31.26285283906726775 ) ) ;
#10492 = CARTESIAN_POINT ( 'NONE',  ( 0.4194150275617615775, 228.8973402254239033, 8.830960608724256033 ) ) ;
#10493 = FACE_BOUND ( 'NONE', #9497, .T. ) ;
#10494 = CARTESIAN_POINT ( 'NONE',  ( -2.500000000000000000, 0.000000000000000000, 2.150000001092474911 ) ) ;
#10495 = CARTESIAN_POINT ( 'NONE',  ( 0.000000000000000000, 184.0000000000000000, -7.000000000000000000 ) ) ;
#10496 = ORIENTED_EDGE ( 'NONE', *, *, #1654, .F. ) ;
#10497 = CARTESIAN_POINT ( 'NONE',  ( -2.066987300000000527, 185.4499999989075150, 7.000000000000000000 ) ) ;
#10498 = CARTESIAN_POINT ( 'NONE',  ( -0.1323933160974937739, 6.000000000000002665, 12.49999999999998757 ) ) ;
#10499 = ORIENTED_EDGE ( 'NONE', *, *, #2916, .F. ) ;
#10500 = DIRECTION ( 'NONE',  ( 0.5877852522924802425, -0.8090169943749422332, 0.000000000000000000 ) ) ;
#10501 = ADVANCED_BREP_SHAPE_REPRESENTATION ( '', ( #5230, #14201 ), #6617 ) ;
#10502 = CARTESIAN_POINT ( 'NONE',  ( -0.8561741729129466183, 184.9999999989074979, 9.066987299999999195 ) ) ;
#10503 = CARTESIAN_POINT ( 'NONE',  ( 5.931828553037980178, 0.9033193133618800941, 17.73805675996853637 ) ) ;
#10504 = CARTESIAN_POINT ( 'NONE',  ( -2.066987300000000527, 186.2499999989074979, 7.000000000000000000 ) ) ;
#10505 = DIRECTION ( 'NONE',  ( -0.9510565162951545304, 0.3090169943749447867, 0.000000000000000000 ) ) ;
#10506 = EDGE_CURVE ( 'NONE', #13817, #5672, #2678, .T. ) ;
#10507 = CARTESIAN_POINT ( 'NONE',  ( 1.035533905932739085, -2.500000000000000000, -1.149999997815050135 ) ) ;
#10508 = CARTESIAN_POINT ( 'NONE',  ( -6.172552660730982410, -0.9821660343538520799, 4.736203831591939917 ) ) ;
#10509 = CARTESIAN_POINT ( 'NONE',  ( 0.000000000000000000, 222.0378120216257400, 12.20449933502084505 ) ) ;
#10510 = DIRECTION ( 'NONE',  ( -0.5877852522924685852, -0.8090169943749507819, 0.000000000000000000 ) ) ;
#10511 = CARTESIAN_POINT ( 'NONE',  ( 4.290381260516270778, 4.545736887716210539, 31.61517780375841369 ) ) ;
#10512 = VECTOR ( 'NONE', #2234, 1000.000000000000000 ) ;
#10513 = CARTESIAN_POINT ( 'NONE',  ( -0.7995298244853260572, -5.947211616899265252, 18.61456014619857058 ) ) ;
#10514 = EDGE_LOOP ( 'NONE', ( #11565, #6366 ) ) ;
#10515 = ADVANCED_FACE ( 'NONE', ( #2339 ), #4739, .F. ) ;
#10516 = EDGE_LOOP ( 'NONE', ( #10874, #13153, #12448, #829 ) ) ;
#10517 = ORIENTED_EDGE ( 'NONE', *, *, #3570, .T. ) ;
#10518 = CARTESIAN_POINT ( 'NONE',  ( 2.996920846510537473, -5.485395142346763286, 12.11441947245483064 ) ) ;
#10519 = DIRECTION ( 'NONE',  ( 0.000000000000000000, 0.000000000000000000, -1.000000000000000000 ) ) ;
#10520 = ORIENTED_EDGE ( 'NONE', *, *, #11555, .T. ) ;
#10521 = CARTESIAN_POINT ( 'NONE',  ( 5.409274167810711909, -2.597759609440523754, 18.61519382448850024 ) ) ;
#10522 = CARTESIAN_POINT ( 'NONE',  ( -1.767766952966369098, 1.767766952966369098, 0.9000000021849495768 ) ) ;
#10523 = CARTESIAN_POINT ( 'NONE',  ( 0.6139908388541017725, -5.969238533166612015, 4.199776279120133182 ) ) ;
#10524 = DIRECTION ( 'NONE',  ( 0.000000000000000000, 0.000000000000000000, 1.000000000000000000 ) ) ;
#10525 = CARTESIAN_POINT ( 'NONE',  ( -1.767766952966369320, 188.1999999978150697, 5.232233047033630235 ) ) ;
#10526 = CARTESIAN_POINT ( 'NONE',  ( 2.500000000000000000, 3.061616997868383141E-16, -1.893000000021849649 ) ) ;
#10527 = CARTESIAN_POINT ( 'NONE',  ( -7.490007020835684592, -2.433650805992431110, 11.49999999999998224 ) ) ;
#10528 = APPLICATION_PROTOCOL_DEFINITION ( 'draft international standard', 'automotive_design', 1998, #3931 ) ;
#10529 = CARTESIAN_POINT ( 'NONE',  ( 2.066987299999999639, 2.531329380823229670E-16, 1.650000001092474911 ) ) ;
#10530 = DIRECTION ( 'NONE',  ( 0.9510565162951499785, 0.3090169943749582204, 0.000000000000000000 ) ) ;
#10531 = CARTESIAN_POINT ( 'NONE',  ( 2.789580270747262780, 227.6450226773988845, 8.373868502673408543 ) ) ;
#10532 = CARTESIAN_POINT ( 'NONE',  ( -0.6829126361173057935, 228.2303005364134094, 10.09526665386122346 ) ) ;
#10533 = VERTEX_POINT ( 'NONE', #990 ) ;
#10534 = CARTESIAN_POINT ( 'NONE',  ( 1.264010580706230957, -2.175748604140837816, -2.499149807554369218 ) ) ;
#10535 = EDGE_LOOP ( 'NONE', ( #5789, #3527 ) ) ;
#10536 = CARTESIAN_POINT ( 'NONE',  ( 3.780072143464286771, -4.979057943639690897, 6.000082193215566129 ) ) ;
#10537 = DIRECTION ( 'NONE',  ( -0.9510565162951545304, 0.3090169943749447867, 0.000000000000000000 ) ) ;
#10538 = CARTESIAN_POINT ( 'NONE',  ( 5.649053410273122466, 2.675685104943152481, 23.88482219624157210 ) ) ;
#10539 = ORIENTED_EDGE ( 'NONE', *, *, #1079, .T. ) ;
#10540 = CARTESIAN_POINT ( 'NONE',  ( -5.903119516422468571, 1.077859910107537678, 17.38480617551147844 ) ) ;
#10541 = CYLINDRICAL_SURFACE ( 'NONE', #7672, 6.250000000000000888 ) ;
#10542 = CARTESIAN_POINT ( 'NONE',  ( 0.000000000000000000, 0.000000000000000000, 0.000000000000000000 ) ) ;
#10543 = CARTESIAN_POINT ( 'NONE',  ( -1.767766952966369098, 1.767766952966369098, 0.7999999999999999334 ) ) ;
#10544 = DIRECTION ( 'NONE',  ( 1.000000000000000000, 0.000000000000000000, 0.000000000000000000 ) ) ;
#10545 = DIRECTION ( 'NONE',  ( 0.000000000000000000, 0.000000000000000000, 1.000000000000000000 ) ) ;
#10546 = CYLINDRICAL_SURFACE ( 'NONE', #9022, 2.500000000000000000 ) ;
#10547 = CARTESIAN_POINT ( 'NONE',  ( -1.767766952966369320, 188.2999999999999829, 5.232233047033630235 ) ) ;
#10548 = CARTESIAN_POINT ( 'NONE',  ( -2.710505431213761085E-17, 228.2551366889530016, 10.16828399152529983 ) ) ;
#10549 = FACE_BOUND ( 'NONE', #4709, .T. ) ;
#10550 = CARTESIAN_POINT ( 'NONE',  ( 2.082642335314403343E-14, -6.250000000000000888, 32.00000000000000000 ) ) ;
#10551 = CARTESIAN_POINT ( 'NONE',  ( -1.524659305057740610E-16, 189.0000000000000000, 4.500000000000000000 ) ) ;
#10552 = B_SPLINE_CURVE_WITH_KNOTS ( 'NONE', 3,
 ( #8409, #14116, #15323, #9433, #6972, #10701, #1071, #9278, #4662, #2102, #15639, #14266, #11730, #9513, #11805, #9352, #2260, #7130 ),
 .UNSPECIFIED., .F., .F.,
 ( 4, 2, 2, 2, 2, 2, 2, 2, 4 ),
 ( 0.003131486019301972078, 0.003522824630466680519, 0.003914163241631389394, 0.004305501852796097401, 0.004696840463960806275, 0.005088179075125516017, 0.005479517686290224891, 0.005870856297454934633, 0.006262194908619643507 ),
 .UNSPECIFIED. ) ;
#10553 = CARTESIAN_POINT ( 'NONE',  ( -1.035533905932739751, 186.1500000000000057, 9.500000000000003553 ) ) ;
#10554 = CARTESIAN_POINT ( 'NONE',  ( -5.131373506000731055, 7.062729720844018289, 31.00000000000000000 ) ) ;
#10556 = ORIENTED_EDGE ( 'NONE', *, *, #15433, .T. ) ;
#10555 = DIRECTION ( 'NONE',  ( -0.9510565162951544194, 0.3090169943749447312, 0.000000000000000000 ) ) ;
#10557 = CARTESIAN_POINT ( 'NONE',  ( -5.984759433606986256, 1.806271833852362008, 19.00008219321555103 ) ) ;
#10558 = VERTEX_POINT ( 'NONE', #12047 ) ;
#10559 = EDGE_CURVE ( 'NONE', #1584, #2087, #8709, .T. ) ;
#10560 = DIRECTION ( 'NONE',  ( 1.000000000000000000, 0.000000000000000000, 0.000000000000000000 ) ) ;
#10561 = CARTESIAN_POINT ( 'NONE',  ( -2.500000000000000444, 184.0000000000000000, 7.000000000000000000 ) ) ;
#10562 = DIRECTION ( 'NONE',  ( -6.123233995736766036E-17, 1.000000000000000000, 0.000000000000000000 ) ) ;
#10563 = FACE_OUTER_BOUND ( 'NONE', #7156, .T. ) ;
#10564 = CARTESIAN_POINT ( 'NONE',  ( -5.621278735166225893, -2.101423246382475352, 5.974080527831013399 ) ) ;
#10565 = CARTESIAN_POINT ( 'NONE',  ( 1.974531203966234827, 228.3459296953993203, 7.238455547615789243 ) ) ;
#10566 = FACE_BOUND ( 'NONE', #1527, .T. ) ;
#10567 = CARTESIAN_POINT ( 'NONE',  ( 0.08288047105113569013, 0.4000000000000045186, 2.550831915580193510 ) ) ;
#10568 = CARTESIAN_POINT ( 'NONE',  ( 0.7988914244718454682, 5.947301735519280541, 30.38456289168619051 ) ) ;
#10569 = EDGE_LOOP ( 'NONE', ( #2710, #12832, #14398, #11061 ) ) ;
#10570 = CARTESIAN_POINT ( 'NONE',  ( 2.066987300000000527, 184.2499999989074979, 7.000000000000000000 ) ) ;
#10571 = CARTESIAN_POINT ( 'NONE',  ( -0.5039079366031817830, 5.980031194523157012, 10.62637068109811622 ) ) ;
#10572 = EDGE_CURVE ( 'NONE', #5999, #9607, #4172, .T. ) ;
#10573 = ORIENTED_EDGE ( 'NONE', *, *, #2981, .F. ) ;
#10574 = FACE_OUTER_BOUND ( 'NONE', #10035, .T. ) ;
#10575 = ADVANCED_FACE ( 'NONE', ( #1069 ), #10779, .F. ) ;
#10576 = CARTESIAN_POINT ( 'NONE',  ( 3.726944967918921492E-17, 185.4499999989075150, 4.933012699999999029 ) ) ;
#10577 = CARTESIAN_POINT ( 'NONE',  ( 4.000000000000002665, 184.0000000000000000, -7.000000000000000888 ) ) ;
#10578 = CARTESIAN_POINT ( 'NONE',  ( 1.461580736456473462, 185.1499999989075320, 5.538419263543526760 ) ) ;
#10579 = CARTESIAN_POINT ( 'NONE',  ( -0.8736772044957569205, 6.188841968496095802, 23.99611573292804678 ) ) ;
#10580 = CARTESIAN_POINT ( 'NONE',  ( -1.530808498934191571E-16, 2.500000000000000000, -0.7999999978150504898 ) ) ;
#10581 = CARTESIAN_POINT ( 'NONE',  ( 2.668367453516645504, -5.373994336898123336, 11.49999999999998224 ) ) ;
#10582 = CARTESIAN_POINT ( 'NONE',  ( -5.999999999999999112, 188.6555110544239824, 3.692234042171783415 ) ) ;
#10583 = CARTESIAN_POINT ( 'NONE',  ( 0.8738043859790958212, -6.188821459035875883, 31.50341560223748161 ) ) ;
#10584 = CARTESIAN_POINT ( 'NONE',  ( 0.8561741729129463963, -2.066987299999999195, -2.299999998907525267 ) ) ;
#10585 = CARTESIAN_POINT ( 'NONE',  ( 6.000000000000000888, 7.347880794884120722E-16, 36.00000000000000711 ) ) ;
#10586 = ORIENTED_EDGE ( 'NONE', *, *, #15632, .F. ) ;
#10587 = EDGE_CURVE ( 'NONE', #2813, #8352, #10854, .T. ) ;
#10588 = ORIENTED_EDGE ( 'NONE', *, *, #10280, .T. ) ;
#10589 = ORIENTED_EDGE ( 'NONE', *, *, #6980, .T. ) ;
#10590 = CARTESIAN_POINT ( 'NONE',  ( 4.069800786343767740, 4.744882212776853514, 30.12618035954928430 ) ) ;
#10591 = CARTESIAN_POINT ( 'NONE',  ( 1.788462153556203305, 228.5496497207740845, 7.826810600328078849 ) ) ;
#10592 = ORIENTED_EDGE ( 'NONE', *, *, #14241, .T. ) ;
#10593 = PRODUCT_DEFINITION_SHAPE ( 'NONE', 'NONE',  #15735 ) ;
#10594 =( BOUNDED_SURFACE ( )  B_SPLINE_SURFACE ( 1, 2, ( 
 ( #11245, #9034, #7667, #269, #7745, #347, #13625, #11326, #504, #15068, #3843, #2972, #10216, #1689, #6566, #4001, #2738, #14834, #9905, #5132, #6413, #2818, #12438, #5211, #10141, #10062, #5294, #12356, #2658, #7823, #4084, #12515, #14759, #14993, #7590, #11401, #3919, #422, #14910, #8878, #1614, #8716, #1538, #5371, #4164, #6490, #13860, #578, #13710, #1770, #12672, #6644, #11474, #8955, #6331, #13549, #12591, #13786, #9984, #7512, #1453, #11168, #9181, #9408, #5754, #11856, #3050, #3353, #15379, #8219, #10525, #5447, #4475, #14172, #11633, #9329, #9257, #12901, #13939, #1924, #10293, #13055, #7901, #15147, #15301, #733, #5677, #10598, #4241, #6877, #811, #1845, #3126, #12743, #7979, #3277, #15459, #4321, #8141, #9110, #6720 ),
 ( #11784, #12976, #8060, #2079, #11553, #14020, #2154, #14244, #6952, #7028, #2002, #649, #5522, #886, #11710, #10369, #15220, #4560, #12820, #6797, #5601, #10447, #4403, #14092, #3202, #10918, #3747, #6074, #7418, #16, #9735, #7187, #4878, #4799, #8465, #9489, #13221, #967, #8623, #14320, #10678, #10833, #12025, #1201, #1281, #15538, #2396, #12101, #13136, #7105, #13458, #9567, #5990, #9810, #2482, #2315, #14573, #14659, #3670, #13299, #4635, #4959, #15615, #10757, #3514, #8383, #7264, #5833, #3428, #11942, #6155, #8547, #2235, #8298, #7341, #4717, #13372, #12183, #2561, #1048, #10994, #14409, #1125, #15695, #5911, #9653, #91, #14494, #3591, #5272, #2718, #251, #13688, #2875, #1671, #6234, #5351, #12572, #4063, #8933, #6392 ) ),
 .UNSPECIFIED., .F., .F., .F. ) 
 B_SPLINE_SURFACE_WITH_KNOTS ( ( 2, 2 ),
 ( 3, 2, 2, 2, 2, 2, 2, 2, 2, 2, 2, 2, 2, 2, 2, 2, 2, 2, 2, 2, 2, 2, 2, 2, 2, 2, 2, 2, 2, 2, 2, 2, 2, 2, 2, 2, 2, 2, 2, 2, 2, 2, 2, 2, 2, 2, 2, 2, 2, 2, 3 ),
 ( 0.000000000000000000, 1.000000000000000000 ),
 ( 0.000000000000000000, 0.01785714285714285615, 0.03571428571428571230, 0.05357142857142856845, 0.07142857142857142461, 0.08928571428571428770, 0.1071428571428571369, 0.1250000000000000000, 0.1428571428571428492, 0.1607142857142857262, 0.1785714285714285754, 0.1964285714285714246, 0.2142857142857142738, 0.2321428571428571508, 0.2500000000000000000, 0.2678571428571428492, 0.2857142857142856984, 0.3035714285714285476, 0.3214285714285714524, 0.3392857142857143016, 0.3571428571428571508, 0.3750000000000000000, 0.3928571428571428492, 0.4107142857142856984, 0.4285714285714285476, 0.4464285714285714524, 0.4642857142857143016, 0.4821428571428571508, 0.5000000000000000000, 0.5178571428571429047, 0.5357142857142856984, 0.5535714285714286031, 0.5714285714285713969, 0.5892857142857143016, 0.6071428571428570953, 0.6250000000000000000, 0.6428571428571429047, 0.6607142857142856984, 0.6785714285714286031, 0.6964285714285713969, 0.7142857142857143016, 0.7321428571428570953, 0.7500000000000000000, 0.7678571428571429047, 0.7857142857142856984, 0.8035714285714286031, 0.8214285714285713969, 0.8392857142857143016, 0.8571428571428570953, 0.8750000000000000000, 0.8928571428571429047 ),
 .UNSPECIFIED. ) 
 GEOMETRIC_REPRESENTATION_ITEM ( )  RATIONAL_B_SPLINE_SURFACE ( (
 ( 1.000000000000000000, 0.9238795325112867385, 1.000000000000000000, 0.9238795325112867385, 1.000000000000000000, 0.9238795325112867385, 1.000000000000000000, 0.9238795325112867385, 1.000000000000000000, 0.9238795325112867385, 1.000000000000000000, 0.9238795325112867385, 1.000000000000000000, 0.9238795325112867385, 1.000000000000000000, 0.9238795325112867385, 1.000000000000000000, 0.9238795325112867385, 1.000000000000000000, 0.9238795325112867385, 1.000000000000000000, 0.9238795325112867385, 1.000000000000000000, 0.9238795325112867385, 1.000000000000000000, 0.9238795325112867385, 1.000000000000000000, 0.9238795325112867385, 1.000000000000000000, 0.9238795325112867385, 1.000000000000000000, 0.9238795325112867385, 1.000000000000000000, 0.9238795325112867385, 1.000000000000000000, 0.9238795325112867385, 1.000000000000000000, 0.9238795325112867385, 1.000000000000000000, 0.9238795325112867385, 1.000000000000000000, 0.9238795325112867385, 1.000000000000000000, 0.9238795325112867385, 1.000000000000000000, 0.9238795325112867385, 1.000000000000000000, 0.9238795325112867385, 1.000000000000000000, 0.9238795325112867385, 1.000000000000000000, 0.9238795325112867385, 1.000000000000000000, 0.9238795325112867385, 1.000000000000000000, 0.9238795325112867385, 1.000000000000000000, 0.9238795325112867385, 1.000000000000000000, 0.9238795325112867385, 1.000000000000000000, 0.9238795325112867385, 1.000000000000000000, 0.9238795325112867385, 1.000000000000000000, 0.9238795325112867385, 1.000000000000000000, 0.9238795325112867385, 1.000000000000000000, 0.9238795325112867385, 1.000000000000000000, 0.9238795325112867385, 1.000000000000000000, 0.9238795325112867385, 1.000000000000000000, 0.9238795325112867385, 1.000000000000000000, 0.9238795325112867385, 1.000000000000000000, 0.9238795325112867385, 1.000000000000000000, 0.9238795325112867385, 1.000000000000000000, 0.9238795325112867385, 1.000000000000000000, 0.9238795325112867385, 1.000000000000000000, 0.9238795325112867385, 1.000000000000000000, 0.9238795325112867385, 1.000000000000000000, 0.9238795325112867385, 1.000000000000000000, 0.9238795325112867385, 1.000000000000000000, 0.9238795325112867385, 1.000000000000000000, 0.9238795325112867385, 1.000000000000000000, 0.9238795325112867385, 1.000000000000000000),
 ( 1.000000000000000000, 0.9238795325112867385, 1.000000000000000000, 0.9238795325112867385, 1.000000000000000000, 0.9238795325112867385, 1.000000000000000000, 0.9238795325112867385, 1.000000000000000000, 0.9238795325112867385, 1.000000000000000000, 0.9238795325112867385, 1.000000000000000000, 0.9238795325112867385, 1.000000000000000000, 0.9238795325112867385, 1.000000000000000000, 0.9238795325112867385, 1.000000000000000000, 0.9238795325112867385, 1.000000000000000000, 0.9238795325112867385, 1.000000000000000000, 0.9238795325112867385, 1.000000000000000000, 0.9238795325112867385, 1.000000000000000000, 0.9238795325112867385, 1.000000000000000000, 0.9238795325112867385, 1.000000000000000000, 0.9238795325112867385, 1.000000000000000000, 0.9238795325112867385, 1.000000000000000000, 0.9238795325112867385, 1.000000000000000000, 0.9238795325112867385, 1.000000000000000000, 0.9238795325112867385, 1.000000000000000000, 0.9238795325112867385, 1.000000000000000000, 0.9238795325112867385, 1.000000000000000000, 0.9238795325112867385, 1.000000000000000000, 0.9238795325112867385, 1.000000000000000000, 0.9238795325112867385, 1.000000000000000000, 0.9238795325112867385, 1.000000000000000000, 0.9238795325112867385, 1.000000000000000000, 0.9238795325112867385, 1.000000000000000000, 0.9238795325112867385, 1.000000000000000000, 0.9238795325112867385, 1.000000000000000000, 0.9238795325112867385, 1.000000000000000000, 0.9238795325112867385, 1.000000000000000000, 0.9238795325112867385, 1.000000000000000000, 0.9238795325112867385, 1.000000000000000000, 0.9238795325112867385, 1.000000000000000000, 0.9238795325112867385, 1.000000000000000000, 0.9238795325112867385, 1.000000000000000000, 0.9238795325112867385, 1.000000000000000000, 0.9238795325112867385, 1.000000000000000000, 0.9238795325112867385, 1.000000000000000000, 0.9238795325112867385, 1.000000000000000000, 0.9238795325112867385, 1.000000000000000000, 0.9238795325112867385, 1.000000000000000000, 0.9238795325112867385, 1.000000000000000000, 0.9238795325112867385, 1.000000000000000000, 0.9238795325112867385, 1.000000000000000000, 0.9238795325112867385, 1.000000000000000000, 0.9238795325112867385, 1.000000000000000000, 0.9238795325112867385, 1.000000000000000000, 0.9238795325112867385, 1.000000000000000000) ) ) 
 REPRESENTATION_ITEM ( '' )  SURFACE ( )  );
#10595 = CARTESIAN_POINT ( 'NONE',  ( 4.592425496802573972E-16, -2.500000000000000000, -1.199999997815050401 ) ) ;
#10596 = CARTESIAN_POINT ( 'NONE',  ( 0.1306497350717338857, -6.000000000000001776, 4.000000000000004441 ) ) ;
#10597 = CARTESIAN_POINT ( 'NONE',  ( 3.568242062701365125, 5.132954954975621931, 25.50004906876533184 ) ) ;
#10598 = CARTESIAN_POINT ( 'NONE',  ( -2.500000000000000444, 189.0499999978150356, 5.964466094067261359 ) ) ;
#10599 = EDGE_CURVE ( 'NONE', #2087, #1584, #6431, .T. ) ;
#10600 = CARTESIAN_POINT ( 'NONE',  ( 2.500000000000000444, 1.035533905932737975, 0.5569999999781504174 ) ) ;
#10601 = AXIS2_PLACEMENT_3D ( 'NONE', #2214, #6855, #1981 ) ;
#10602 = CARTESIAN_POINT ( 'NONE',  ( -25.39999999999994884, 6.000306541065368193E-16, -1.500000000000001776 ) ) ;
#10603 = CARTESIAN_POINT ( 'NONE',  ( -2.066987299999999639, 0.8561741729129452860, 0.4000000010924749105 ) ) ;
#10604 = CARTESIAN_POINT ( 'NONE',  ( 2.500000000000000444, 187.9699999975965738, 7.000000000000000000 ) ) ;
#10605 = CARTESIAN_POINT ( 'NONE',  ( 2.733135974173155791, 227.6887743597950760, 8.502598298417593625 ) ) ;
#10606 = EDGE_CURVE ( 'NONE', #3644, #6042, #5740, .T. ) ;
#10607 = CARTESIAN_POINT ( 'NONE',  ( 4.069684453406205549, 4.744965295353637202, 18.87380055247394850 ) ) ;
#10608 = ORIENTED_EDGE ( 'NONE', *, *, #6498, .F. ) ;
#10609 = CARTESIAN_POINT ( 'NONE',  ( -1.767766952966369542, 185.9999999978150527, 8.767766952966368876 ) ) ;
#10610 = AXIS2_PLACEMENT_3D ( 'NONE', #2743, #7593, #5216 ) ;
#10611 = ORIENTED_EDGE ( 'NONE', *, *, #10220, .F. ) ;
#10612 = CARTESIAN_POINT ( 'NONE',  ( 0.000000000000000000, 184.0000000000000000, 7.000000000000000000 ) ) ;
#10613 = AXIS2_PLACEMENT_3D ( 'NONE', #1258, #3805, #13276 ) ;
#10614 = CYLINDRICAL_SURFACE ( 'NONE', #714, 1.000000000000000666 ) ;
#10615 = CARTESIAN_POINT ( 'NONE',  ( -0.7993282387951125001, 5.947240459526509149, 5.614843582169575242 ) ) ;
#10616 = ORIENTED_EDGE ( 'NONE', *, *, #2375, .T. ) ;
#10617 = CARTESIAN_POINT ( 'NONE',  ( 5.131373506000584506, 7.062729720844102665, 31.00000000000000000 ) ) ;
#10618 = UNCERTAINTY_MEASURE_WITH_UNIT (LENGTH_MEASURE( 1.000000000000000082E-05 ), #14072, 'distance_accuracy_value', 'NONE');
#10619 = CARTESIAN_POINT ( 'NONE',  ( 5.409423237179077582, -2.597448116730894263, 17.38438267301393481 ) ) ;
#10620 = DIRECTION ( 'NONE',  ( 0.5877852522924802425, -0.8090169943749422332, 0.000000000000000000 ) ) ;
#10621 = CARTESIAN_POINT ( 'NONE',  ( -2.500000000000000000, 0.000000000000000000, -1.399999997815050357 ) ) ;
#10622 = CARTESIAN_POINT ( 'NONE',  ( -2.500000000000000000, 0.000000000000000000, 0.9000000000000000222 ) ) ;
#10623 = CARTESIAN_POINT ( 'NONE',  ( -6.176542424588095770, -0.9554180641287001174, 11.49999999999998224 ) ) ;
#10624 =( NAMED_UNIT ( * ) PLANE_ANGLE_UNIT ( ) SI_UNIT ( $, .RADIAN. ) );
#10625 = VECTOR ( 'NONE', #2709, 1000.000000000000000 ) ;
#10626 = DIRECTION ( 'NONE',  ( -0.3090169943749579429, 0.9510565162951502005, 0.000000000000000000 ) ) ;
#10627 = CARTESIAN_POINT ( 'NONE',  ( -2.500000000000000444, 188.3499999999999943, 5.964466094067261359 ) ) ;
#10628 = AXIS2_PLACEMENT_3D ( 'NONE', #2296, #9715, #149 ) ;
#10629 = CARTESIAN_POINT ( 'NONE',  ( 0.6320692372082544752, 228.2335842258707430, 10.10492066627648988 ) ) ;
#10630 = CARTESIAN_POINT ( 'NONE',  ( 5.746619684944269224, 1.730157667110847397, 10.49995067926686154 ) ) ;
#10631 = CARTESIAN_POINT ( 'NONE',  ( 5.931793676715084729, 0.9035324301689270365, 31.26239891805597537 ) ) ;
#10632 = CARTESIAN_POINT ( 'NONE',  ( 1.767766952966368432, 188.7000000000000171, 8.767766952966368876 ) ) ;
#10633 = FACE_OUTER_BOUND ( 'NONE', #3817, .T. ) ;
#10635 = EDGE_LOOP ( 'NONE', ( #3139, #1836 ) ) ;
#10634 = DIRECTION ( 'NONE',  ( 0.000000000000000000, 0.000000000000000000, -1.000000000000000000 ) ) ;
#10636 = LINE ( 'NONE', #15256, #12469 ) ;
#10637 = AXIS2_PLACEMENT_3D ( 'NONE', #14212, #8105, #692 ) ;
#10638 = CARTESIAN_POINT ( 'NONE',  ( -2.066987299999999639, 0.8561741729129452860, 2.200000001092475177 ) ) ;
#10639 = CARTESIAN_POINT ( 'NONE',  ( -2.585318580472420802, 226.7961291864880877, 5.874574987694232142 ) ) ;
#10640 = CARTESIAN_POINT ( 'NONE',  ( 1.035533905932739085, -2.500000000000000000, -0.3499999978150501456 ) ) ;
#10641 = CARTESIAN_POINT ( 'NONE',  ( 2.500000000000000444, 183.9300000002185129, 7.000000000000000000 ) ) ;
#10642 = CARTESIAN_POINT ( 'NONE',  ( -4.435347140101077557, 4.403429997944469321, 5.130639327542137806 ) ) ;
#10643 = CARTESIAN_POINT ( 'NONE',  ( 1.884974866327016940, 228.4701649684375866, 7.597254102066775872 ) ) ;
#10644 = FACE_BOUND ( 'NONE', #8926, .T. ) ;
#10645 = CARTESIAN_POINT ( 'NONE',  ( 0.8561741729129465073, -2.066987299999999195, 1.700000001092474733 ) ) ;
#10646 = FACE_OUTER_BOUND ( 'NONE', #13250, .T. ) ;
#10647 = ORIENTED_EDGE ( 'NONE', *, *, #13016, .F. ) ;
#10648 = CARTESIAN_POINT ( 'NONE',  ( 2.066987300000000527, 187.4499999989075150, 7.000000000000000000 ) ) ;
#10649 = EDGE_CURVE ( 'NONE', #8460, #9974, #1112, .T. ) ;
#10650 = DIRECTION ( 'NONE',  ( 1.000000000000000000, 0.000000000000000000, 0.000000000000000000 ) ) ;
#10651 = ORIENTED_EDGE ( 'NONE', *, *, #8550, .F. ) ;
#10652 = CARTESIAN_POINT ( 'NONE',  ( 1.767766952966368432, 186.2999999999999829, 8.767766952966368876 ) ) ;
#10653 = MECHANICAL_DESIGN_GEOMETRIC_PRESENTATION_REPRESENTATION (  '', ( #3282 ), #1508 ) ;
#10654 = PRESENTATION_LAYER_ASSIGNMENT (  '', '', ( #11677 ) ) ;
#10655 = CARTESIAN_POINT ( 'NONE',  ( 2.500000000000000444, 1.035533905932737975, -0.1499999978150502455 ) ) ;
#10656 = CARTESIAN_POINT ( 'NONE',  ( 2.817313151350985034, 5.579000502529534167, 17.99999999999998934 ) ) ;
#10657 = CARTESIAN_POINT ( 'NONE',  ( 2.066987300000000527, 185.0999999989075206, 6.143825827087054492 ) ) ;
#10658 = CARTESIAN_POINT ( 'NONE',  ( 4.286401442266576822, -4.198423832313147308, 30.86760611998364112 ) ) ;
#10659 = CARTESIAN_POINT ( 'NONE',  ( 4.592425496802573972E-16, -2.500000000000000000, -0.3999999978150502455 ) ) ;
#10660 = CARTESIAN_POINT ( 'NONE',  ( 3.107278289587213749, -5.134157760522037428, 10.62635295315575767 ) ) ;
#10661 = CARTESIAN_POINT ( 'NONE',  ( 5.999999999999999112, 201.6409668649147022, 13.30942870683726120 ) ) ;
#10662 = CARTESIAN_POINT ( 'NONE',  ( 1.767766952966369098, 188.7999999978150356, 5.232233047033630235 ) ) ;
#10663 = CARTESIAN_POINT ( 'NONE',  ( 2.500000000000000000, 3.061616997868383141E-16, 2.500000000000000000 ) ) ;
#10664 = CARTESIAN_POINT ( 'NONE',  ( 5.665707375537457402, 1.979196487016721573, 12.50007961174474858 ) ) ;
#10665 = ADVANCED_FACE ( 'NONE', ( #9757 ), #12439, .T. ) ;
#10666 = ORIENTED_EDGE ( 'NONE', *, *, #9996, .T. ) ;
#10667 =( GEOMETRIC_REPRESENTATION_CONTEXT ( 3 ) GLOBAL_UNCERTAINTY_ASSIGNED_CONTEXT ( ( #675 ) ) GLOBAL_UNIT_ASSIGNED_CONTEXT ( ( #4499, #10624, #8322 ) ) REPRESENTATION_CONTEXT ( 'NONE', 'WORKASPACE' ) );
#10668 = ADVANCED_FACE ( 'NONE', ( #6254 ), #2741, .F. ) ;
#10669 = ORIENTED_EDGE ( 'NONE', *, *, #14948, .T. ) ;
#10670 = ORIENTED_EDGE ( 'NONE', *, *, #553, .T. ) ;
#10671 = CARTESIAN_POINT ( 'NONE',  ( 4.195795028114968517, -4.289273350251384898, 25.00428920362019625 ) ) ;
#10672 = CARTESIAN_POINT ( 'NONE',  ( 0.5202723921993107625, 228.8949738520769586, 8.824126387528728799 ) ) ;
#10673 = EDGE_CURVE ( 'NONE', #12720, #5458, #15130, .T. ) ;
#10674 = ORIENTED_EDGE ( 'NONE', *, *, #9620, .T. ) ;
#10675 = CARTESIAN_POINT ( 'NONE',  ( -1.461580736456472351, -1.461580736456473018, 1.350000001092474644 ) ) ;
#10676 = CARTESIAN_POINT ( 'NONE',  ( -5.746837578675995317, -1.729433780394289188, 31.99995053646223653 ) ) ;
#10677 = CARTESIAN_POINT ( 'NONE',  ( 4.286401442266388528, 4.198423832313340043, 24.49999999999999289 ) ) ;
#10678 = CARTESIAN_POINT ( 'NONE',  ( -2.066987300000000083, 186.4499999989075150, 7.000000000000000000 ) ) ;
#10679 = CARTESIAN_POINT ( 'NONE',  ( -2.500000000000000000, -1.035533905932739307, -1.443000000021849694 ) ) ;
#10680 =( BOUNDED_CURVE ( )  B_SPLINE_CURVE ( 2, ( #728, #4399, #9253, #14087, #12894, #6332, #710, #11169, #3920 ),
 .UNSPECIFIED., .F., .F. ) 
 B_SPLINE_CURVE_WITH_KNOTS ( ( 3, 2, 2, 2, 3 ),
 ( 0.1428571428571428492, 0.1607142857142857539, 0.1785714285714286031, 0.1964285714285714524, 0.2142857142857143293 ),
 .UNSPECIFIED. ) 
 CURVE ( )  GEOMETRIC_REPRESENTATION_ITEM ( )  RATIONAL_B_SPLINE_CURVE ( ( 1.000000000000000000, 0.9238795325112867385, 1.000000000000000000, 0.9238795325112867385, 1.000000000000000000, 0.9238795325112867385, 1.000000000000000000, 0.9238795325112865164, 1.000000000000000222 ) ) 
 REPRESENTATION_ITEM ( '' )  );
#10681 = CARTESIAN_POINT ( 'NONE',  ( 2.897581130414634077E-17, -9.750000000000003553, 0.000000000000000000 ) ) ;
#10682 = CARTESIAN_POINT ( 'NONE',  ( -1.265664690411614835E-16, 2.066987299999999639, -0.5499999989075254891 ) ) ;
#10683 = B_SPLINE_CURVE_WITH_KNOTS ( 'NONE', 3,
 ( #12785, #13827, #695, #5337, #11364, #1734, #15111, #4209, #10415, #15265, #9079, #6609, #4366, #2781, #2940, #10180, #4047, #11442 ),
 .UNSPECIFIED., .F., .F.,
 ( 4, 2, 2, 2, 2, 2, 2, 2, 4 ),
 ( 0.000000000000000000, 0.0003914357524127484072, 0.0007828715048254968143, 0.001174307257238245330, 0.001565743009650993629, 0.001957178762063741927, 0.002348614514476490660, 0.002740050266889238959, 0.003131486019301987257 ),
 .UNSPECIFIED. ) ;
#10684 = CARTESIAN_POINT ( 'NONE',  ( 13.50000000000000000, 0.000000000000000000, -8.673617379884035472E-16 ) ) ;
#10685 = CARTESIAN_POINT ( 'NONE',  ( 1.980782313704909203, 226.5644727820218520, 5.192016377768971402 ) ) ;
#10686 = CARTESIAN_POINT ( 'NONE',  ( 4.344313232727004426, 4.493553492990209897, 18.50436969680152899 ) ) ;
#10687 = ORIENTED_EDGE ( 'NONE', *, *, #10232, .T. ) ;
#10688 = CARTESIAN_POINT ( 'NONE',  ( 1.035533905932738419, 186.1499999978150584, 9.500000000000000000 ) ) ;
#10689 = ORIENTED_EDGE ( 'NONE', *, *, #12897, .T. ) ;
#10690 = ORIENTED_EDGE ( 'NONE', *, *, #2387, .F. ) ;
#10691 = CARTESIAN_POINT ( 'NONE',  ( -6.081509788407712058, 1.446521464462830142, 25.37381964045071214 ) ) ;
#10692 = CARTESIAN_POINT ( 'NONE',  ( 3.011899281037397458, -5.190111395030288399, 17.19977782616120265 ) ) ;
#10693 = CARTESIAN_POINT ( 'NONE',  ( 0.1306394121199382363, -6.250000000000000888, 4.000000000000005329 ) ) ;
#10694 = ORIENTED_EDGE ( 'NONE', *, *, #8523, .T. ) ;
#10695 = CARTESIAN_POINT ( 'NONE',  ( -5.570820891630815730, 2.833901239560305818, 31.26236973443877076 ) ) ;
#10696 = FACE_OUTER_BOUND ( 'NONE', #5101, .T. ) ;
#10697 = EDGE_CURVE ( 'NONE', #7319, #1678, #4728, .T. ) ;
#10698 = CARTESIAN_POINT ( 'NONE',  ( -0.9737725088280243524, -6.173885267451852954, 24.23735758726565592 ) ) ;
#10699 = CARTESIAN_POINT ( 'NONE',  ( -4.344502777243604896, 4.493369211529193663, 12.00389213124967114 ) ) ;
#10700 = CARTESIAN_POINT ( 'NONE',  ( 0.9999502950803423884, -5.916088184763861335, 18.13108149190010465 ) ) ;
#10701 = CARTESIAN_POINT ( 'NONE',  ( -4.154121946521006414, -4.670585111242854914, 25.29887838423338309 ) ) ;
#10702 = DIRECTION ( 'NONE',  ( 1.000000000000000000, 0.000000000000000000, 0.000000000000000000 ) ) ;
#10703 = CARTESIAN_POINT ( 'NONE',  ( 0.02384593234141434148, 0.4000000000000097367, -2.517027090855607607 ) ) ;
#10704 = ADVANCED_FACE ( 'NONE', ( #1690 ), #13940, .F. ) ;
#10705 = CARTESIAN_POINT ( 'NONE',  ( -1.035533905932737975, 186.5499999978150640, 4.500000000000000888 ) ) ;
#10706 = CARTESIAN_POINT ( 'NONE',  ( 1.583222688839772019, 228.1098062731747689, 9.740983991995673108 ) ) ;
#10707 = CARTESIAN_POINT ( 'NONE',  ( 5.571002711501477300, -2.833546409886150030, 17.73620383159192571 ) ) ;
#10708 = CARTESIAN_POINT ( 'NONE',  ( -1.398763622202980894, 189.4255937783873094, 4.329173634885357558 ) ) ;
#10709 = EDGE_CURVE ( 'NONE', #1252, #28, #580, .T. ) ;
#10710 = ORIENTED_EDGE ( 'NONE', *, *, #5465, .F. ) ;
#10711 = CARTESIAN_POINT ( 'NONE',  ( -4.286401442266592809, 4.198423832313131321, 5.000000000000004441 ) ) ;
#10712 = CYLINDRICAL_SURFACE ( 'NONE', #12254, 1.000000000000000888 ) ;
#10714 = ORIENTED_EDGE ( 'NONE', *, *, #10406, .F. ) ;
#10713 = CYLINDRICAL_SURFACE ( 'NONE', #11318, 2.500000000000000000 ) ;
#10715 = FACE_OUTER_BOUND ( 'NONE', #5441, .T. ) ;
#10716 = CARTESIAN_POINT ( 'NONE',  ( 0.09128442572436945568, 0.4000000000000010214, 2.551849451885215725 ) ) ;
#10717 = ORIENTED_EDGE ( 'NONE', *, *, #6297, .T. ) ;
#10718 = DIRECTION ( 'NONE',  ( 0.000000000000000000, 0.000000000000000000, 1.000000000000000000 ) ) ;
#10719 = CARTESIAN_POINT ( 'NONE',  ( -1.461580736456472351, -1.461580736456473018, 0.7500000010924748883 ) ) ;
#10720 = CARTESIAN_POINT ( 'NONE',  ( -2.999416585479811381, 227.3092116331243631, 7.385563965123170149 ) ) ;
#10721 = CYLINDRICAL_SURFACE ( 'NONE', #1626, 1.499999999999999556 ) ;
#10722 = CARTESIAN_POINT ( 'NONE',  ( 1.767766952966369320, 185.6300000002185016, 5.232233047033630235 ) ) ;
#10723 = CARTESIAN_POINT ( 'NONE',  ( -0.0007128680628333008105, 227.6089742637946642, 5.110086227958842819 ) ) ;
#10724 = CARTESIAN_POINT ( 'NONE',  ( 0.9965032137571403492, 227.6963699622695287, 5.362489989878645780 ) ) ;
#10725 = CARTESIAN_POINT ( 'NONE',  ( 0.000000000000000000, 0.000000000000000000, 53.67766952966368876 ) ) ;
#10726 = CARTESIAN_POINT ( 'NONE',  ( 1.461580736456472573, 1.461580736456472795, -0.4499999989075252338 ) ) ;
#10727 = CARTESIAN_POINT ( 'NONE',  ( 6.143143148203063397, 1.154591847827682871, 17.38603820591927729 ) ) ;
#10728 = EDGE_LOOP ( 'NONE', ( #3232, #14293 ) ) ;
#10729 = CARTESIAN_POINT ( 'NONE',  ( 0.000000000000000000, 2.000000000000000000, -11.50000000000000000 ) ) ;
#10730 = PRODUCT_DEFINITION_SHAPE ( 'NONE', 'NONE',  #15752 ) ;
#10731 = CARTESIAN_POINT ( 'NONE',  ( 2.066987300000000971, 185.8999999989075036, 6.143825827087054492 ) ) ;
#10732 = CYLINDRICAL_SURFACE ( 'NONE', #11883, 1.000000000000000888 ) ;
#10733 = ORIENTED_EDGE ( 'NONE', *, *, #8936, .T. ) ;
#10734 = DIRECTION ( 'NONE',  ( -0.000000000000000000, 1.000000000000000000, -0.000000000000000000 ) ) ;
#10735 = CARTESIAN_POINT ( 'NONE',  ( -4.435347140101121965, 4.403429997944421359, 11.49999999999998224 ) ) ;
#10736 = CARTESIAN_POINT ( 'NONE',  ( -3.735642931251060617, 4.696778275484448706, 31.97408052783100985 ) ) ;
#10737 = DIRECTION ( 'NONE',  ( 0.000000000000000000, 0.000000000000000000, 1.000000000000000000 ) ) ;
#10738 = CARTESIAN_POINT ( 'NONE',  ( 0.000000000000000000, 186.0499999989075093, 4.933012699999999029 ) ) ;
#10739 = CARTESIAN_POINT ( 'NONE',  ( 4.286401442266577710, -4.198423832313146420, 31.00000000000000000 ) ) ;
#10740 = CARTESIAN_POINT ( 'NONE',  ( 2.500000000000000444, 1.035533905932737975, -1.749999997815050667 ) ) ;
#10741 = DIRECTION ( 'NONE',  ( -1.000000000000000000, 0.000000000000000000, 0.000000000000000000 ) ) ;
#10742 = CARTESIAN_POINT ( 'NONE',  ( 0.07162589071487505954, 189.0001276426230561, 4.501026264287848910 ) ) ;
#10743 = CARTESIAN_POINT ( 'NONE',  ( -5.931817299736853677, 0.9033986943601943764, 11.23770962164068976 ) ) ;
#10744 = CARTESIAN_POINT ( 'NONE',  ( 1.767766952966368654, 185.3999999978150584, 8.767766952966368876 ) ) ;
#10745 = CARTESIAN_POINT ( 'NONE',  ( -0.2624013748571840110, -5.995472630654527180, 17.02628559691081733 ) ) ;
#10746 = ORIENTED_EDGE ( 'NONE', *, *, #14068, .F. ) ;
#10747 = AXIS2_PLACEMENT_3D ( 'NONE', #1148, #13552, #6096 ) ;
#10748 = ORIENTED_EDGE ( 'NONE', *, *, #7650, .T. ) ;
#10749 = ORIENTED_EDGE ( 'NONE', *, *, #12609, .F. ) ;
#10750 = B_SPLINE_CURVE_WITH_KNOTS ( 'NONE', 3,
 ( #3373, #8240, #10389, #13074, #11879, #989, #5853, #10698, #7916, #4340, #4659, #9197, #6093, #15636, #5052, #112, #8406, #13394 ),
 .UNSPECIFIED., .F., .F.,
 ( 4, 2, 2, 2, 2, 2, 2, 2, 4 ),
 ( 0.003131490185286093120, 0.003522829482338693183, 0.003914168779391293679, 0.004305508076443894175, 0.004696847373496493804, 0.005088186670549094300, 0.005479525967601693928, 0.005870865264654294424, 0.006262204561706894920 ),
 .UNSPECIFIED. ) ;
#10751 = CARTESIAN_POINT ( 'NONE',  ( -2.668367453516768517, 5.373994336898062052, 11.49999999999998224 ) ) ;
#10752 = EDGE_LOOP ( 'NONE', ( #8850, #12971 ) ) ;
#10753 = CARTESIAN_POINT ( 'NONE',  ( 2.500000000000000444, 1.035533905932737975, -1.749999997815050889 ) ) ;
#10754 = EDGE_CURVE ( 'NONE', #12097, #15371, #8467, .T. ) ;
#10755 = LINE ( 'NONE', #5675, #8846 ) ;
#10756 = CARTESIAN_POINT ( 'NONE',  ( 2.999999999999999556, -1.732050807568877859, -5.500000000000000000 ) ) ;
#10757 = CARTESIAN_POINT ( 'NONE',  ( 2.066987299999999639, 187.5999999989075491, 7.856174172912946396 ) ) ;
#10758 = VECTOR ( 'NONE', #1113, 1000.000000000000000 ) ;
#10759 = CARTESIAN_POINT ( 'NONE',  ( 4.592425496802573972E-16, -2.500000000000000000, -1.293000000021849338 ) ) ;
#10760 = EDGE_CURVE ( 'NONE', #2054, #13232, #14995, .T. ) ;
#10761 = CARTESIAN_POINT ( 'NONE',  ( 5.649200442566173486, -2.675373855294116865, 4.384398071070796377 ) ) ;
#10762 = ITEM_DEFINED_TRANSFORMATION ( 'NONE', 'NONE', #13909,  #14201 ) ;
#10763 = CARTESIAN_POINT ( 'NONE',  ( -1.461580736456472351, -1.461580736456473018, -1.049999998907525489 ) ) ;
#10764 = CARTESIAN_POINT ( 'NONE',  ( 2.930922878467574488, -5.520395124723521896, 30.49610786875030044 ) ) ;
#10765 = CARTESIAN_POINT ( 'NONE',  ( 0.1966278158245924057, 226.3267328078643459, 4.491244098638222937 ) ) ;
#10766 = CARTESIAN_POINT ( 'NONE',  ( 5.558508435838189321, 2.857531096718932240, 5.000000000000004441 ) ) ;
#10767 = ORIENTED_EDGE ( 'NONE', *, *, #3829, .T. ) ;
#10768 = VERTEX_POINT ( 'NONE', #7902 ) ;
#10769 = CARTESIAN_POINT ( 'NONE',  ( -2.500000000000001776, 188.3499999978150470, 8.035533905932737753 ) ) ;
#10770 = VERTEX_POINT ( 'NONE', #10295 ) ;
#10771 = VERTEX_POINT ( 'NONE', #9035 ) ;
#10772 = CARTESIAN_POINT ( 'NONE',  ( -6.176542424588101987, -0.9554180641286524889, 31.00000000000000000 ) ) ;
#10773 = CARTESIAN_POINT ( 'NONE',  ( -3.255128505894383739, -5.336774832660674761, 23.62619944752604439 ) ) ;
#10774 = CARTESIAN_POINT ( 'NONE',  ( -25.39999999999994884, -4.163336342344337027E-16, 1.500000000000001776 ) ) ;
#10775 = CARTESIAN_POINT ( 'NONE',  ( -5.558508435838179551, -2.857531096718951336, 31.00000000000000000 ) ) ;
#10776 = EDGE_CURVE ( 'NONE', #2165, #1532, #6511, .T. ) ;
#10777 = CARTESIAN_POINT ( 'NONE',  ( -0.8738239080080343335, -6.188820299975591688, 5.503557957101422815 ) ) ;
#10778 = CYLINDRICAL_SURFACE ( 'NONE', #12242, 12.50000000000000533 ) ;
#10779 = CYLINDRICAL_SURFACE ( 'NONE', #3187, 2.000000000000000000 ) ;
#10780 = CARTESIAN_POINT ( 'NONE',  ( 5.531796221294850824, 2.326749136277279639, 30.12621569129737864 ) ) ;
#10781 = CARTESIAN_POINT ( 'NONE',  ( 0.1323933160977649182, -5.999999999999995559, 25.49999999999999289 ) ) ;
#10782 = DIRECTION ( 'NONE',  ( -1.000000000000000000, 0.000000000000000000, 0.000000000000000000 ) ) ;
#10783 = CARTESIAN_POINT ( 'NONE',  ( -2.500000000000000444, 186.7499999978150242, 8.035533905932737753 ) ) ;
#10784 = CARTESIAN_POINT ( 'NONE',  ( 2.975657739721877970, 227.4162173224905530, 7.700537803285528504 ) ) ;
#10785 = CARTESIAN_POINT ( 'NONE',  ( -5.570722351696197450, -2.834100162822098756, 18.26190213084011660 ) ) ;
#10786 = CARTESIAN_POINT ( 'NONE',  ( 0.8499999999999896527, -0.3999999999999906408, -2.750000000000010658 ) ) ;
#10787 = EDGE_LOOP ( 'NONE', ( #2557, #324 ) ) ;
#10788 = DIRECTION ( 'NONE',  ( 0.000000000000000000, 0.000000000000000000, 1.000000000000000000 ) ) ;
#10789 = CARTESIAN_POINT ( 'NONE',  ( -0.7988914244717549851, -5.947301735519293864, 10.88456289168616742 ) ) ;
#10790 = ORIENTED_EDGE ( 'NONE', *, *, #12054, .T. ) ;
#10791 = LINE ( 'NONE', #12657, #12414 ) ;
#10792 = CARTESIAN_POINT ( 'NONE',  ( 2.682774040342114308, 226.8574465069323765, 6.055224137038854870 ) ) ;
#10793 = CARTESIAN_POINT ( 'NONE',  ( 4.344265632481963735, 4.493596842505074740, 23.99574050496988775 ) ) ;
#10794 = VECTOR ( 'NONE', #10510, 1000.000000000000114 ) ;
#10795 = CARTESIAN_POINT ( 'NONE',  ( 3.796994071234844259E-16, -2.066987299999999639, -0.7499999989075251117 ) ) ;
#10796 = CARTESIAN_POINT ( 'NONE',  ( -2.891600564906900317, 227.0306417089624347, 6.565254640817405729 ) ) ;
#10797 = ADVANCED_FACE ( 'NONE', ( #11402 ), #5807, .T. ) ;
#10798 = CARTESIAN_POINT ( 'NONE',  ( 3.061616997868383141E-16, 2.000000000000000000, 2.500000000000000000 ) ) ;
#10799 = CARTESIAN_POINT ( 'NONE',  ( -1.767766952966369320, 188.2300000002184959, 5.232233047033630235 ) ) ;
#10800 = CARTESIAN_POINT ( 'NONE',  ( -3.458467055437274063, 5.207305717053841043, 5.973595717233013858 ) ) ;
#10801 = CARTESIAN_POINT ( 'NONE',  ( -1.288813234857717038, 227.7638191499166851, 5.557287090853593625 ) ) ;
#10802 = CARTESIAN_POINT ( 'NONE',  ( 5.984377695197225400, 1.807429553002283029, 10.49995093123465217 ) ) ;
#10803 = CARTESIAN_POINT ( 'NONE',  ( -0.8561741729129455081, 2.066987299999999639, 2.100000001092475088 ) ) ;
#10804 = CARTESIAN_POINT ( 'NONE',  ( -3.000000000000000000, 1.732050807568877415, -5.500000000000000000 ) ) ;
#10805 = EDGE_CURVE ( 'NONE', #8352, #260, #15392, .T. ) ;
#10806 = VERTEX_POINT ( 'NONE', #13514 ) ;
#10807 = CARTESIAN_POINT ( 'NONE',  ( -1.461580736456473240, 188.5499999989075093, 5.538419263543526760 ) ) ;
#10808 = CARTESIAN_POINT ( 'NONE',  ( 0.8561741729129457301, 186.7999999989074809, 4.933012699999999029 ) ) ;
#10809 = CARTESIAN_POINT ( 'NONE',  ( 5.935543223013877601, 0.8771126767605439412, 24.36935038651144581 ) ) ;
#10810 = B_SPLINE_CURVE_WITH_KNOTS ( 'NONE', 3,
 ( #8689, #157, #5020, #2469, #12091, #2386, #8372, #14483, #4867, #1269, #4, #14561, #8613, #3657, #3736, #10823, #1116, #6296 ),
 .UNSPECIFIED., .F., .F.,
 ( 4, 2, 2, 2, 2, 2, 2, 2, 4 ),
 ( 0.000000000000000000, 0.0003914898357794965736, 0.0007829796715589933641, 0.001174469507338490046, 0.001565959343117987162, 0.001957449178897483627, 0.002348939014676980092, 0.002740428850456476557, 0.003131918686235973456 ),
 .UNSPECIFIED. ) ;
#10811 = AXIS2_PLACEMENT_3D ( 'NONE', #13318, #15637, #9350 ) ;
#10812 = VERTEX_POINT ( 'NONE', #4780 ) ;
#10813 = CARTESIAN_POINT ( 'NONE',  ( 1.000049271338691481, -6.169473353325520826, 24.36969612704551125 ) ) ;
#10814 = CARTESIAN_POINT ( 'NONE',  ( -4.322356511625772058, 7.650514973136511188, 5.000000000000004441 ) ) ;
#10815 = CYLINDRICAL_SURFACE ( 'NONE', #13416, 1.000000000000000888 ) ;
#10816 = CARTESIAN_POINT ( 'NONE',  ( -0.8561741729129470624, 187.9999999989075263, 9.066987300000000971 ) ) ;
#10817 = CARTESIAN_POINT ( 'NONE',  ( 2.668367453516690357, -5.373994336898101132, 31.00000000000000000 ) ) ;
#10818 = CARTESIAN_POINT ( 'NONE',  ( 0.6408967059908734498, 188.9999999999627391, 9.420550830048384228 ) ) ;
#10819 = CARTESIAN_POINT ( 'NONE',  ( 5.935543223013876712, 0.8771126767605440522, 24.49999999999999289 ) ) ;
#10820 = CARTESIAN_POINT ( 'NONE',  ( 5.935543223013864278, -0.8771126767606430841, 31.13064961348856130 ) ) ;
#10821 = CARTESIAN_POINT ( 'NONE',  ( -2.500000000000000444, 1.035533905932737753, 0.8500000000000001998 ) ) ;
#10822 = DIRECTION ( 'NONE',  ( 1.000000000000000000, 0.000000000000000000, 0.000000000000000000 ) ) ;
#10823 = CARTESIAN_POINT ( 'NONE',  ( -5.329907877631385738, 2.755840666746196543, 30.73805675996854703 ) ) ;
#10824 = VERTEX_POINT ( 'NONE', #9636 ) ;
#10825 = ORIENTED_EDGE ( 'NONE', *, *, #923, .F. ) ;
#10826 = ORIENTED_EDGE ( 'NONE', *, *, #11157, .F. ) ;
#10827 = CARTESIAN_POINT ( 'NONE',  ( 1.938790558398429731, 228.4312510197253800, 7.484868398679935808 ) ) ;
#10828 = ORIENTED_EDGE ( 'NONE', *, *, #8234, .F. ) ;
#10829 = PRODUCT_DEFINITION_SHAPE ( 'NONE', 'NONE',  #2335 ) ;
#10830 = CARTESIAN_POINT ( 'NONE',  ( -2.500000000000000000, 0.000000000000000000, -2.999999997815050889 ) ) ;
#10831 = CARTESIAN_POINT ( 'NONE',  ( 5.558508435838253270, 2.857531096718811892, 17.99999999999998934 ) ) ;
#10832 = CARTESIAN_POINT ( 'NONE',  ( 6.143020266950968811, 1.155160780047759683, 31.61441947245484485 ) ) ;
#10833 = CARTESIAN_POINT ( 'NONE',  ( -2.066987300000000971, 186.4999999989075263, 7.856174172912944620 ) ) ;
#10834 = CARTESIAN_POINT ( 'NONE',  ( -1.530808498934191571E-16, 2.500000000000000000, 0.7069999999781503286 ) ) ;
#10835 = LINE ( 'NONE', #1128, #7191 ) ;
#10836 = CONTEXT_DEPENDENT_SHAPE_REPRESENTATION ( #6514, #11996 ) ;
#10837 = CARTESIAN_POINT ( 'NONE',  ( 2.066987300000000083, -0.8561741729129449530, -2.399999998907525356 ) ) ;
#10838 = CYLINDRICAL_SURFACE ( 'NONE', #2512, 1.000000000000000666 ) ;
#10839 = CARTESIAN_POINT ( 'NONE',  ( -2.842542329930219491, 227.5997332721124451, 8.240608773874100734 ) ) ;
#10840 = CARTESIAN_POINT ( 'NONE',  ( 6.155973317223274677, 1.081218830693777777, 5.503086438660448998 ) ) ;
#10841 = EDGE_LOOP ( 'NONE', ( #15498, #1174 ) ) ;
#10842 = EDGE_LOOP ( 'NONE', ( #4552, #1387, #1970, #14563 ) ) ;
#10843 = CARTESIAN_POINT ( 'NONE',  ( -1.767766952966369765, 188.3999999978150584, 8.767766952966368876 ) ) ;
#10844 = VERTEX_POINT ( 'NONE', #2381 ) ;
#10845 = ORIENTED_EDGE ( 'NONE', *, *, #11186, .F. ) ;
#10846 = EDGE_CURVE ( 'NONE', #645, #9042, #5016, .T. ) ;
#10847 = CARTESIAN_POINT ( 'NONE',  ( -5.984759433606997803, -1.806271833852329145, 29.99991780678443476 ) ) ;
#10848 = FACE_BOUND ( 'NONE', #9973, .T. ) ;
#10849 = CARTESIAN_POINT ( 'NONE',  ( 6.176542424588136626, 0.9554180641284277797, 24.49999999999999289 ) ) ;
#10850 = EDGE_CURVE ( 'NONE', #8014, #12563, #13083, .T. ) ;
#10851 = CARTESIAN_POINT ( 'NONE',  ( -5.558508435838219519, 2.857531096718872732, 31.00000000000000000 ) ) ;
#10852 = DIRECTION ( 'NONE',  ( -1.000000000000000000, 0.000000000000000000, 0.000000000000000000 ) ) ;
#10853 = CARTESIAN_POINT ( 'NONE',  ( -3.736532060717985715, -4.696070028785973349, 12.47377823943291908 ) ) ;
#10854 = LINE ( 'NONE', #15720, #11060 ) ;
#10855 = CARTESIAN_POINT ( 'NONE',  ( -5.858813228503575665, -2.179803269293471679, 23.52622717124730656 ) ) ;
#10856 = FACE_OUTER_BOUND ( 'NONE', #8635, .T. ) ;
#10857 = DIRECTION ( 'NONE',  ( 0.000000000000000000, 0.000000000000000000, 1.000000000000000000 ) ) ;
#10858 = PRODUCT_DEFINITION_SHAPE ( 'NONE', 'NONE',  #15750 ) ;
#10859 = CARTESIAN_POINT ( 'NONE',  ( -1.767766952966369765, 188.3999999978150584, 8.767766952966368876 ) ) ;
#10860 = CARTESIAN_POINT ( 'NONE',  ( 0.1966278158245924057, 226.3267328078643459, 4.491244098638222937 ) ) ;
#10861 = AXIS2_PLACEMENT_3D ( 'NONE', #6417, #15072, #13629 ) ;
#10862 = CARTESIAN_POINT ( 'NONE',  ( 5.317509234263964046, 2.779225709350989337, 11.36760611998364823 ) ) ;
#10863 =( REPRESENTATION_RELATIONSHIP ('NONE','NONE', #11191, #3059 ) REPRESENTATION_RELATIONSHIP_WITH_TRANSFORMATION ( #3432 )SHAPE_REPRESENTATION_RELATIONSHIP( ) );
#10864 = AXIS2_PLACEMENT_3D ( 'NONE', #13370, #7416, #7490 ) ;
#10865 = ADVANCED_FACE ( 'NONE', ( #1497 ), #3569, .T. ) ;
#10866 = CARTESIAN_POINT ( 'NONE',  ( -0.8324916443616545703, 189.0000000018762307, 4.635459683989287427 ) ) ;
#10867 = ORIENTED_EDGE ( 'NONE', *, *, #6103, .T. ) ;
#10868 = CARTESIAN_POINT ( 'NONE',  ( -4.006441409774724960, 4.467329318258222770, 4.201117577520601998 ) ) ;
#10869 = LINE ( 'NONE', #1156, #5407 ) ;
#10871 = EDGE_LOOP ( 'NONE', ( #8398, #9249, #13368, #4927 ) ) ;
#10870 = DIRECTION ( 'NONE',  ( -6.123233995736766036E-17, 1.000000000000000000, 0.000000000000000000 ) ) ;
#10872 = FACE_OUTER_BOUND ( 'NONE', #13910, .T. ) ;
#10873 = DIRECTION ( 'NONE',  ( 0.000000000000000000, 0.9449569463142380998, -0.3271946967975951637 ) ) ;
#10874 = ORIENTED_EDGE ( 'NONE', *, *, #11819, .F. ) ;
#10875 = VECTOR ( 'NONE', #3362, 1000.000000000000000 ) ;
#10876 = CARTESIAN_POINT ( 'NONE',  ( -2.066987299999999639, 0.000000000000000000, 2.150000001092474911 ) ) ;
#10877 = VECTOR ( 'NONE', #11672, 1000.000000000000114 ) ;
#10878 = CARTESIAN_POINT ( 'NONE',  ( -2.066987299999999639, 0.000000000000000000, -0.9499999989075252893 ) ) ;
#10879 = CARTESIAN_POINT ( 'NONE',  ( -0.001074311305641557088, 226.3251817249170017, 4.486671161788877704 ) ) ;
#10880 =( NAMED_UNIT ( * ) PLANE_ANGLE_UNIT ( ) SI_UNIT ( $, .RADIAN. ) );
#10881 = CARTESIAN_POINT ( 'NONE',  ( -1.000082492230699671, -6.169467968613712827, 31.13152538105391542 ) ) ;
#10882 = CARTESIAN_POINT ( 'NONE',  ( 1.767766952966369098, 188.8300000002184902, 5.232233047033630235 ) ) ;
#10883 = DIRECTION ( 'NONE',  ( 0.000000000000000000, 1.000000000000000000, 0.000000000000000000 ) ) ;
#10884 = CARTESIAN_POINT ( 'NONE',  ( 1.940097806574041073, 228.1129668193434838, 6.565645474235799917 ) ) ;
#10885 = CARTESIAN_POINT ( 'NONE',  ( -0.8561741729129455081, 2.066987299999999639, -0.2999999989075252671 ) ) ;
#10886 = B_SPLINE_CURVE_WITH_KNOTS ( 'NONE', 1,
 ( #11656, #8164 ),
 .UNSPECIFIED., .F., .F.,
 ( 2, 2 ),
 ( 0.000000000000000000, 1.000000000000000000 ),
 .UNSPECIFIED. ) ;
#10887 = CARTESIAN_POINT ( 'NONE',  ( 1.035533905932737531, 2.500000000000000444, 1.450000000000000400 ) ) ;
#10888 = ORIENTED_EDGE ( 'NONE', *, *, #3118, .T. ) ;
#10889 = CARTESIAN_POINT ( 'NONE',  ( 0.8561741729129456191, 188.3999999989075036, 4.933012699999999029 ) ) ;
#10890 = VECTOR ( 'NONE', #5515, 1000.000000000000114 ) ;
#10891 = CARTESIAN_POINT ( 'NONE',  ( -0.8561741729129471734, 187.1999999989075434, 9.066987300000000971 ) ) ;
#10892 = CARTESIAN_POINT ( 'NONE',  ( 5.317509234264027107, 2.779225709350867213, 24.49999999999999289 ) ) ;
#10893 = VERTEX_POINT ( 'NONE', #9294 ) ;
#10894 = ADVANCED_FACE ( 'NONE', ( #3320 ), #14285, .F. ) ;
#10895 = CARTESIAN_POINT ( 'NONE',  ( 0.000000000000000000, 0.000000000000000000, -20.00000000000000000 ) ) ;
#10896 = LINE ( 'NONE', #12081, #3489 ) ;
#10897 = CARTESIAN_POINT ( 'NONE',  ( 5.558508435838239059, -2.857531096718835428, 31.00000000000000000 ) ) ;
#10898 = DIRECTION ( 'NONE',  ( -0.3090169943749579429, 0.9510565162951502005, 0.000000000000000000 ) ) ;
#10899 = CARTESIAN_POINT ( 'NONE',  ( -1.461580736456473906, 188.7499999989075263, 8.461580736456474128 ) ) ;
#10900 = CARTESIAN_POINT ( 'NONE',  ( 3.922288969639839085, -4.542045818322474560, 30.12621569129737864 ) ) ;
#10901 = CARTESIAN_POINT ( 'NONE',  ( -2.066987299999999639, 0.8561741729129452860, -0.9999999989075254447 ) ) ;
#10902 = CARTESIAN_POINT ( 'NONE',  ( 1.038438449965593646, 189.0000000004559979, 9.278652163284620613 ) ) ;
#10903 = DIRECTION ( 'NONE',  ( 0.000000000000000000, 0.000000000000000000, 1.000000000000000000 ) ) ;
#10904 = CARTESIAN_POINT ( 'NONE',  ( -2.283493650000000041, 0.000000000000000000, 2.375000000546237278 ) ) ;
#10905 = CARTESIAN_POINT ( 'NONE',  ( -0.8738239080078950005, -6.188820299975613004, 18.50355795710142104 ) ) ;
#10906 = CARTESIAN_POINT ( 'NONE',  ( 5.843075991566563765, 1.368655265451134140, 4.126352953155773662 ) ) ;
#10907 = CARTESIAN_POINT ( 'NONE',  ( 5.317509234263963158, 2.779225709350988449, 11.49999999999998224 ) ) ;
#10908 = ORIENTED_EDGE ( 'NONE', *, *, #1432, .F. ) ;
#10909 = EDGE_LOOP ( 'NONE', ( #4412, #5714, #4568, #7969 ) ) ;
#10910 = ORIENTED_EDGE ( 'NONE', *, *, #15329, .T. ) ;
#10911 = EDGE_CURVE ( 'NONE', #3363, #7505, #6248, .T. ) ;
#10912 = DIRECTION ( 'NONE',  ( -0.9510565162951545304, 0.3090169943749447867, 0.000000000000000000 ) ) ;
#10913 = VERTEX_POINT ( 'NONE', #8183 ) ;
#10914 = EDGE_CURVE ( 'NONE', #5531, #6066, #13422, .T. ) ;
#10915 = CARTESIAN_POINT ( 'NONE',  ( -2.066987299999999639, 0.000000000000000000, 1.250000001092474777 ) ) ;
#10916 = DIRECTION ( 'NONE',  ( -0.5000000000000000000, -0.8660254037844387076, 0.000000000000000000 ) ) ;
#10917 = CARTESIAN_POINT ( 'NONE',  ( 5.985119669071097270, 1.805077827356622588, 31.99991741810289625 ) ) ;
#10918 = CARTESIAN_POINT ( 'NONE',  ( -2.066987300000000971, 185.6999999989075434, 7.856174172912944620 ) ) ;
#10919 = CARTESIAN_POINT ( 'NONE',  ( -2.500000000000000000, -1.035533905932739307, 0.1499999999999999667 ) ) ;
#10920 = CARTESIAN_POINT ( 'NONE',  ( -5.782947755040681592, 1.603807858343930137, 31.97398020122239259 ) ) ;
#10921 = CARTESIAN_POINT ( 'NONE',  ( -1.461580736456472795, 1.461580736456472795, 1.350000001092474644 ) ) ;
#10922 = CARTESIAN_POINT ( 'NONE',  ( -2.932912173331216898, 227.0860177055994882, 6.728427774621575708 ) ) ;
#10923 = CARTESIAN_POINT ( 'NONE',  ( 2.126728311762493650E-16, 19.99999999999999645, 8.250000000000003553 ) ) ;
#10924 = VERTEX_POINT ( 'NONE', #6916 ) ;
#10925 = ORIENTED_EDGE ( 'NONE', *, *, #7022, .F. ) ;
#10926 = LINE ( 'NONE', #15040, #10625 ) ;
#10927 = ORIENTED_EDGE ( 'NONE', *, *, #5703, .T. ) ;
#10928 = ORIENTED_EDGE ( 'NONE', *, *, #11585, .F. ) ;
#10929 = CARTESIAN_POINT ( 'NONE',  ( -6.176542424588088664, 0.9554180641287480791, 24.49999999999999289 ) ) ;
#10930 = CARTESIAN_POINT ( 'NONE',  ( 2.782468714962326395, -5.316055268221460572, 17.49610204984018225 ) ) ;
#10931 =( GEOMETRIC_REPRESENTATION_CONTEXT ( 3 ) GLOBAL_UNCERTAINTY_ASSIGNED_CONTEXT ( ( #8006 ) ) GLOBAL_UNIT_ASSIGNED_CONTEXT ( ( #8244, #13078, #3148 ) ) REPRESENTATION_CONTEXT ( 'NONE', 'WORKASPACE' ) );
#10932 = CARTESIAN_POINT ( 'NONE',  ( -4.286401442266677186, -4.198423832313046944, 24.63061695532137918 ) ) ;
#10933 = CARTESIAN_POINT ( 'NONE',  ( -5.317509234263907203, 2.779225709351096807, 17.86935038651143159 ) ) ;
#10934 = B_SPLINE_CURVE_WITH_KNOTS ( 'NONE', 3,
 ( #11433, #8992, #8828, #7544, #6598, #5483, #1571, #1801, #13894, #13581, #303, #610, #12626, #10327, #1724, #1489, #535, #15103 ),
 .UNSPECIFIED., .F., .F.,
 ( 4, 2, 2, 2, 2, 2, 2, 2, 4 ),
 ( 0.000000000000000000, 0.0003914898357794968447, 0.0007829796715589936893, 0.001174469507338490480, 0.001565959343117987379, 0.001957449178897484061, 0.002348939014676980960, 0.002740428850456477858, 0.003131918686235974757 ),
 .UNSPECIFIED. ) ;
#10935 = CARTESIAN_POINT ( 'NONE',  ( 3.779681992289718906, -4.979315417303956437, 23.50004921015706216 ) ) ;
#10936 = FACE_OUTER_BOUND ( 'NONE', #226, .T. ) ;
#10937 = CARTESIAN_POINT ( 'NONE',  ( -5.558508435838229289, 2.857531096718854524, 5.000000000000004441 ) ) ;
#10938 = CARTESIAN_POINT ( 'NONE',  ( -5.558508435838094286, -2.857531096719115205, 24.36939309276500154 ) ) ;
#10939 = DIRECTION ( 'NONE',  ( 0.9510565162951499785, 0.3090169943749582204, 0.000000000000000000 ) ) ;
#10940 = DIRECTION ( 'NONE',  ( 0.000000000000000000, 1.000000000000000000, 0.000000000000000000 ) ) ;
#10941 = CARTESIAN_POINT ( 'NONE',  ( -2.500000000000000888, 188.2999999978150356, 7.000000000000000000 ) ) ;
#10942 = CARTESIAN_POINT ( 'NONE',  ( 2.999966428792078865, 227.3061007205240571, 7.376404775963534277 ) ) ;
#10943 = CARTESIAN_POINT ( 'NONE',  ( 5.375886393124366336, 2.665038680141326832, 10.99560239355786528 ) ) ;
#10944 = CARTESIAN_POINT ( 'NONE',  ( -2.088929602433466037, 189.4018337869057405, 4.846696350498261197 ) ) ;
#10945 = ORIENTED_EDGE ( 'NONE', *, *, #4965, .T. ) ;
#10946 = CARTESIAN_POINT ( 'NONE',  ( 0.000000000000000000, 0.000000000000000000, 2.500000000000000000 ) ) ;
#10947 = CARTESIAN_POINT ( 'NONE',  ( 6.780834053290958173E-14, -6.000000000000000888, 10.49999999999998224 ) ) ;
#10948 = CARTESIAN_POINT ( 'NONE',  ( 1.035533905932738197, 187.8500000000000227, 9.500000000000000000 ) ) ;
#10949 = CARTESIAN_POINT ( 'NONE',  ( 4.416397290909964468, -4.422724436066375553, 31.26379616840806008 ) ) ;
#10950 = B_SPLINE_CURVE_WITH_KNOTS ( 'NONE', 3,
 ( #868, #12959, #15361, #4457, #1903, #11531, #12724, #12652, #13919, #4302, #712, #10348, #9164, #8041, #3107, #3183, #10272, #559 ),
 .UNSPECIFIED., .F., .F.,
 ( 4, 2, 2, 2, 2, 2, 2, 2, 4 ),
 ( 0.003131918686235979094, 0.003523310662250268930, 0.003914702638264559199, 0.004306094614278849035, 0.004697486590293138871, 0.005088878566307429574, 0.005480270542321719410, 0.005871662518336009245, 0.006263054494350299081 ),
 .UNSPECIFIED. ) ;
#10951 = CARTESIAN_POINT ( 'NONE',  ( 0.000000000000000000, 228.2633636156256216, 6.999999999969752196 ) ) ;
#10952 = CARTESIAN_POINT ( 'NONE',  ( -3.736532060718054993, 4.696070028785918282, 10.52622176056704895 ) ) ;
#10953 = CARTESIAN_POINT ( 'NONE',  ( -1.461580736456472351, -1.461580736456473018, -0.8499999989075254225 ) ) ;
#10954 = DIRECTION ( 'NONE',  ( 0.000000000000000000, 0.000000000000000000, 1.000000000000000000 ) ) ;
#10955 = EDGE_CURVE ( 'NONE', #11668, #5344, #3196, .T. ) ;
#10956 = CARTESIAN_POINT ( 'NONE',  ( 2.094888799673178700E-14, -6.250000000000000888, 30.00000000000000000 ) ) ;
#10957 = CARTESIAN_POINT ( 'NONE',  ( 1.767766952966369098, 188.0300000002185072, 5.232233047033630235 ) ) ;
#10958 = CARTESIAN_POINT ( 'NONE',  ( -2.817313151351189315, 5.579000502529433803, 5.132374107163055754 ) ) ;
#10959 = ADVANCED_FACE ( 'NONE', ( #5874 ), #10721, .F. ) ;
#10960 = CARTESIAN_POINT ( 'NONE',  ( 1.452733574390970395, 228.7063250495755540, 8.279297886081021574 ) ) ;
#10961 = CARTESIAN_POINT ( 'NONE',  ( 2.066987299999999639, 2.531329380823229670E-16, 0.2500000010924748328 ) ) ;
#10962 = CARTESIAN_POINT ( 'NONE',  ( 5.558508435838253270, 2.857531096718811892, 17.86762589283693359 ) ) ;
#10963 = EDGE_CURVE ( 'NONE', #14081, #2165, #5565, .T. ) ;
#10964 = VERTEX_POINT ( 'NONE', #10798 ) ;
#10965 = CARTESIAN_POINT ( 'NONE',  ( 1.461580736456473240, 189.1499999989075036, 5.538419263543526760 ) ) ;
#10966 = CARTESIAN_POINT ( 'NONE',  ( -2.066987300000000971, 186.9999999989074979, 6.143825827087054492 ) ) ;
#10967 = DIRECTION ( 'NONE',  ( 0.000000000000000000, 1.000000000000000000, 0.000000000000000000 ) ) ;
#10969 = EDGE_LOOP ( 'NONE', ( #5288, #7016 ) ) ;
#10968 = CARTESIAN_POINT ( 'NONE',  ( 4.286401442266448036, -4.198423832313277870, 24.49999999999999289 ) ) ;
#10970 = SURFACE_SIDE_STYLE ('',( #12159 ) ) ;
#10971 = CARTESIAN_POINT ( 'NONE',  ( -2.500000000000000444, 184.0000000000000000, 7.000000000000000000 ) ) ;
#10972 = CARTESIAN_POINT ( 'NONE',  ( 4.322356511625649489, 7.650514973136559149, 5.000000000000004441 ) ) ;
#10973 = CARTESIAN_POINT ( 'NONE',  ( 0.8738239080080689725, 6.188820299975588135, 12.00355795710146012 ) ) ;
#10974 = CARTESIAN_POINT ( 'NONE',  ( -0.8561741729129458411, 188.4999999989075263, 4.933012699999999029 ) ) ;
#10975 = CARTESIAN_POINT ( 'NONE',  ( 2.668367453516584220, -5.373994336898154422, 17.99999999999998934 ) ) ;
#10976 = CARTESIAN_POINT ( 'NONE',  ( -0.07135113763453347635, 189.0441085615117345, 10.18309864254113961 ) ) ;
#10977 = CARTESIAN_POINT ( 'NONE',  ( -0.8730424326980719130, -5.936362132114466839, 30.49500690218564358 ) ) ;
#10978 = B_SPLINE_CURVE_WITH_KNOTS ( 'NONE', 3,
 ( #8140, #5832, #7978, #12819, #12975, #8297, #14319, #13135, #11783, #10597, #15458, #11552, #1923, #4559, #6796, #11632, #14717, #71 ),
 .UNSPECIFIED., .F., .F.,
 ( 4, 2, 2, 2, 2, 2, 2, 2, 4 ),
 ( 0.000000000000000000, 0.0003914357524127492203, 0.0007828715048254984406, 0.001174307257238247715, 0.001565743009650996014, 0.001957178762063745397, 0.002348614514476494129, 0.002740050266889243729, 0.003131486019301992895 ),
 .UNSPECIFIED. ) ;
#10979 = CARTESIAN_POINT ( 'NONE',  ( 5.843318061569068966, -1.367618216965539979, 10.62696220972947003 ) ) ;
#10980 = CARTESIAN_POINT ( 'NONE',  ( 6.176542424588149949, -0.9554180641283412934, 24.49999999999999289 ) ) ;
#10981 = CARTESIAN_POINT ( 'NONE',  ( -6.155867707731114358, 1.081837891425874831, 10.99563030319846924 ) ) ;
#10982 = DIRECTION ( 'NONE',  ( 1.000000000000000000, 0.000000000000000000, 0.000000000000000000 ) ) ;
#10983 = ORIENTED_EDGE ( 'NONE', *, *, #11076, .F. ) ;
#10984 = VERTEX_POINT ( 'NONE', #11986 ) ;
#10985 = EDGE_LOOP ( 'NONE', ( #10130, #7995, #2070, #15469 ) ) ;
#10986 = AXIS2_PLACEMENT_3D ( 'NONE', #8580, #12214, #13253 ) ;
#10987 = CARTESIAN_POINT ( 'NONE',  ( -4.286401442266737583, 4.198423832312984771, 24.49999999999999289 ) ) ;
#10988 = ORIENTED_EDGE ( 'NONE', *, *, #13811, .T. ) ;
#10989 = EDGE_CURVE ( 'NONE', #8520, #15586, #4330, .T. ) ;
#10990 = PRODUCT_DEFINITION_SHAPE ( 'NONE', 'NONE',  #15730 ) ;
#10991 = CARTESIAN_POINT ( 'NONE',  ( 1.035533905932739085, -2.500000000000000000, -1.949999997815050401 ) ) ;
#10992 = DIRECTION ( 'NONE',  ( 0.000000000000000000, 0.000000000000000000, -1.000000000000000000 ) ) ;
#10993 = CARTESIAN_POINT ( 'NONE',  ( -1.768703179866833342, 189.0000639513403939, 5.233169770031948609 ) ) ;
#10994 = CARTESIAN_POINT ( 'NONE',  ( 2.066987299999999639, 188.4499999989075150, 7.000000000000000000 ) ) ;
#10995 = CARTESIAN_POINT ( 'NONE',  ( -1.767766952966368432, -1.767766952966369320, 1.000000000000000000 ) ) ;
#10996 = CARTESIAN_POINT ( 'NONE',  ( 0.000000000000000000, 184.0000000000000000, -7.000000000000000000 ) ) ;
#10997 = CARTESIAN_POINT ( 'NONE',  ( 3.632753594129320085, 4.777047695050985254, 5.999950536462231199 ) ) ;
#10998 = CARTESIAN_POINT ( 'NONE',  ( 2.066987299999999639, 0.8561741729129456191, 1.900000001092474688 ) ) ;
#10999 = EDGE_CURVE ( 'NONE', #13850, #10806, #132, .T. ) ;
#11000 = CIRCLE ( 'NONE', #4135, 1.000000000000000888 ) ;
#11001 = CARTESIAN_POINT ( 'NONE',  ( 4.290381260516340056, -4.545736887716145702, 4.384822196241565884 ) ) ;
#11002 = CARTESIAN_POINT ( 'NONE',  ( -1.942272232823049061, 226.5542875158922129, 5.161998670295230518 ) ) ;
#11003 = CYLINDRICAL_SURFACE ( 'NONE', #11550, 5.000000000000000000 ) ;
#11004 = EDGE_LOOP ( 'NONE', ( #2865, #13270 ) ) ;
#11005 = ORIENTED_EDGE ( 'NONE', *, *, #1450, .F. ) ;
#11006 = ORIENTED_EDGE ( 'NONE', *, *, #3939, .F. ) ;
#11007 = CARTESIAN_POINT ( 'NONE',  ( -0.05280746222630467585, 189.0001365486126303, 9.499442212161147481 ) ) ;
#11008 = CARTESIAN_POINT ( 'NONE',  ( 2.996920846510521930, 5.485395142346772168, 4.385580527545153373 ) ) ;
#11009 = LINE ( 'NONE', #8401, #6082 ) ;
#11010 = CARTESIAN_POINT ( 'NONE',  ( 2.692335458626911482, -5.362264153667202216, 11.76239891805595938 ) ) ;
#11011 = CARTESIAN_POINT ( 'NONE',  ( 8.250000000000003553, -1.019131563299854308E-13, 0.000000000000000000 ) ) ;
#11012 = CARTESIAN_POINT ( 'NONE',  ( -2.668367453516692134, -5.373994336898101132, 11.63236078583908473 ) ) ;
#11013 = CARTESIAN_POINT ( 'NONE',  ( -5.648794263291788909, 2.676232015153523935, 5.614419472454846627 ) ) ;
#11014 = CARTESIAN_POINT ( 'NONE',  ( -6.020865209844544097, -1.681180471732322435, 23.52599901976669727 ) ) ;
#11015 = CYLINDRICAL_SURFACE ( 'NONE', #6942, 2.500000000000000444 ) ;
#11016 = DIRECTION ( 'NONE',  ( 0.000000000000000000, -1.000000000000000000, 0.000000000000000000 ) ) ;
#11017 = B_SPLINE_CURVE_WITH_KNOTS ( 'NONE', 3,
 ( #5092, #13584, #537, #4203, #3009 ),
 .UNSPECIFIED., .F., .F.,
 ( 4, 1, 4 ),
 ( 0.009490796809568564224, 0.009530342151606398249, 0.009569887493644234008 ),
 .UNSPECIFIED. ) ;
#11018 = CARTESIAN_POINT ( 'NONE',  ( -2.500000000000000888, 189.0999999978150470, 7.000000000000000000 ) ) ;
#11019 = CARTESIAN_POINT ( 'NONE',  ( 1.980782313704909203, 226.5644727820218520, 5.192016377768971402 ) ) ;
#11020 = CARTESIAN_POINT ( 'NONE',  ( 5.843075991566577088, 1.368655265451070413, 10.62635295315575057 ) ) ;
#11021 = VECTOR ( 'NONE', #10337, 1000.000000000000000 ) ;
#11022 = CARTESIAN_POINT ( 'NONE',  ( -2.084265404442477987, 189.7627086689134330, 9.536083203068468350 ) ) ;
#11023 = B_SPLINE_CURVE_WITH_KNOTS ( 'NONE', 3,
 ( #2724, #14822, #9971, #14979, #8704, #2647, #8940, #7653, #9893, #8862, #7423, #14897, #7576, #3984, #334, #12423, #3907, #1523 ),
 .UNSPECIFIED., .F., .F.,
 ( 4, 2, 2, 2, 2, 2, 2, 2, 4 ),
 ( 0.003131486019302005472, 0.003522824630466710009, 0.003914163241631414547, 0.004305501852796119952, 0.004696840463960824490, 0.005088179075125529027, 0.005479517686290232698, 0.005870856297454936368, 0.006262194908619640905 ),
 .UNSPECIFIED. ) ;
#11024 = EDGE_LOOP ( 'NONE', ( #5646, #3853, #13559, #4391 ) ) ;
#11025 = LINE ( 'NONE', #45, #6336 ) ;
#11026 = CARTESIAN_POINT ( 'NONE',  ( -7.490007020835699691, -2.433650805992386701, 31.00000000000000000 ) ) ;
#11027 = CARTESIAN_POINT ( 'NONE',  ( 5.783198643800800731, 1.602922020054582397, 25.47377823943293151 ) ) ;
#11028 = CARTESIAN_POINT ( 'NONE',  ( 0.2624013748575224625, 5.995472630654511192, 23.52628559691082799 ) ) ;
#11029 = CARTESIAN_POINT ( 'NONE',  ( 1.487915498575067774, 226.4497023322808218, 4.853725831513067135 ) ) ;
#11030 = CARTESIAN_POINT ( 'NONE',  ( 3.780072143464055401, 4.979057943639872974, 23.49991780678443476 ) ) ;
#11031 = CARTESIAN_POINT ( 'NONE',  ( 2.066987299999999639, 2.531329380823229670E-16, 1.050000001092474822 ) ) ;
#11032 = CARTESIAN_POINT ( 'NONE',  ( -2.817313151351372724, 5.579000502529338767, 24.49999999999999289 ) ) ;
#11033 = PRESENTATION_STYLE_ASSIGNMENT (( #7305 ) ) ;
#11034 = CARTESIAN_POINT ( 'NONE',  ( -7.799024015210642702, -1.482594289697281020, 11.49999999999998224 ) ) ;
#11035 = CARTESIAN_POINT ( 'NONE',  ( 2.500000000000000444, 186.3800000002185016, 5.964466094067262247 ) ) ;
#11036 = DIRECTION ( 'NONE',  ( 0.000000000000000000, 0.000000000000000000, -1.000000000000000000 ) ) ;
#11037 = CARTESIAN_POINT ( 'NONE',  ( 1.986724198295925836, 228.2179917342068052, 6.868963418589798309 ) ) ;
#11038 = DIRECTION ( 'NONE',  ( 0.000000000000000000, 0.000000000000000000, 1.000000000000000000 ) ) ;
#11039 = CARTESIAN_POINT ( 'NONE',  ( 2.500000000000000444, 1.035533905932737975, 1.350000000000000089 ) ) ;
#11040 = ORIENTED_EDGE ( 'NONE', *, *, #3699, .T. ) ;
#11041 = CARTESIAN_POINT ( 'NONE',  ( 1.461580736456473018, -1.461580736456472573, 0.7500000010924746663 ) ) ;
#11042 = CARTESIAN_POINT ( 'NONE',  ( 2.066987300000000083, 185.7999999989075093, 7.856174172912946396 ) ) ;
#11043 = CARTESIAN_POINT ( 'NONE',  ( 5.746619684944315409, 1.730157667110706399, 23.49995067926686687 ) ) ;
#11045 = ORIENTED_EDGE ( 'NONE', *, *, #210, .T. ) ;
#11044 = CARTESIAN_POINT ( 'NONE',  ( 1.461580736456472573, 185.1499999989075320, 8.461580736456474128 ) ) ;
#11046 = ADVANCED_FACE ( 'NONE', ( #12147 ), #14699, .T. ) ;
#11047 = CARTESIAN_POINT ( 'NONE',  ( -2.782713018890741186, -5.315928322779106097, 23.99560239355786351 ) ) ;
#11048 = CARTESIAN_POINT ( 'NONE',  ( 2.031800923367348393E-13, -6.250000000000000888, 23.49999999999999289 ) ) ;
#11049 = FACE_OUTER_BOUND ( 'NONE', #8540, .T. ) ;
#11050 = CARTESIAN_POINT ( 'NONE',  ( 0.000000000000000000, 187.2933328889893687, 9.583808270834989429 ) ) ;
#11051 = CARTESIAN_POINT ( 'NONE',  ( -2.273135563902617839, 189.0000000000000568, 8.047421711106334641 ) ) ;
#11052 = CARTESIAN_POINT ( 'NONE',  ( -2.500000000000000000, -1.035533905932739307, 0.1499999999999999944 ) ) ;
#11053 = CARTESIAN_POINT ( 'NONE',  ( -2.500000000000000000, -1.035533905932739307, -2.149999997815051245 ) ) ;
#11054 = CARTESIAN_POINT ( 'NONE',  ( -0.9999196734182431712, -5.916093360767519016, 30.86725955955067136 ) ) ;
#11055 = CARTESIAN_POINT ( 'NONE',  ( 5.665707375537482271, -1.979196487016652961, 10.49992038825522123 ) ) ;
#11056 = CARTESIAN_POINT ( 'NONE',  ( -1.767766952966369098, 1.767766952966369098, -2.299999997815050712 ) ) ;
#11057 = CARTESIAN_POINT ( 'NONE',  ( -5.935543223013816316, -0.8771126767609508379, 24.49999999999999289 ) ) ;
#11058 = FACE_OUTER_BOUND ( 'NONE', #8049, .T. ) ;
#11059 = ORIENTED_EDGE ( 'NONE', *, *, #15431, .T. ) ;
#11060 = VECTOR ( 'NONE', #4820, 1000.000000000000000 ) ;
#11061 = ORIENTED_EDGE ( 'NONE', *, *, #10195, .T. ) ;
#11062 = EDGE_CURVE ( 'NONE', #2943, #5672, #5075, .T. ) ;
#11063 = ORIENTED_EDGE ( 'NONE', *, *, #15629, .F. ) ;
#11064 = CARTESIAN_POINT ( 'NONE',  ( -5.935543223013816316, -0.8771126767609506159, 24.63239388001634111 ) ) ;
#11065 = ORIENTED_EDGE ( 'NONE', *, *, #51, .F. ) ;
#11066 = CARTESIAN_POINT ( 'NONE',  ( -0.8561741729129455081, 2.066987299999999639, 0.3000000010924747662 ) ) ;
#11067 = EDGE_CURVE ( 'NONE', #202, #546, #8663, .T. ) ;
#11068 = CARTESIAN_POINT ( 'NONE',  ( 0.000000000000000000, 182.0000000000000000, 0.000000000000000000 ) ) ;
#11069 = CARTESIAN_POINT ( 'NONE',  ( -13.50000000000000000, 0.000000000000000000, 2.479909768273400161E-15 ) ) ;
#11070 = DIRECTION ( 'NONE',  ( 0.000000000000000000, 0.000000000000000000, -1.000000000000000000 ) ) ;
#11071 = CARTESIAN_POINT ( 'NONE',  ( -1.530808498934191571E-16, 2.500000000000000000, -2.493000000021849516 ) ) ;
#11072 =( REPRESENTATION_RELATIONSHIP ('NONE','NONE', #11191, #4596 ) REPRESENTATION_RELATIONSHIP_WITH_TRANSFORMATION ( #3751 )SHAPE_REPRESENTATION_RELATIONSHIP( ) );
#11073 = CARTESIAN_POINT ( 'NONE',  ( 2.668367453516568677, 5.373994336898162416, 11.49999999999998224 ) ) ;
#11074 = FACE_BOUND ( 'NONE', #14943, .T. ) ;
#11075 = CARTESIAN_POINT ( 'NONE',  ( 3.796994071234844259E-16, -2.066987299999999639, -2.549999998907525267 ) ) ;
#11076 = EDGE_CURVE ( 'NONE', #8963, #902, #2597, .T. ) ;
#11077 = LINE ( 'NONE', #10128, #4033 ) ;
#11078 = CARTESIAN_POINT ( 'NONE',  ( -2.994031302066835654, 227.3524127508109132, 7.512731884239616242 ) ) ;
#11079 = ORIENTED_EDGE ( 'NONE', *, *, #13770, .F. ) ;
#11080 = ORIENTED_EDGE ( 'NONE', *, *, #4237, .F. ) ;
#11081 = ORIENTED_EDGE ( 'NONE', *, *, #12512, .T. ) ;
#11082 = CARTESIAN_POINT ( 'NONE',  ( -2.668367453516725885, 5.373994336898083368, 31.00000000000000000 ) ) ;
#11083 = CARTESIAN_POINT ( 'NONE',  ( -1.500000000000000000, -9.750000000000003553, 2.000000000000001776 ) ) ;
#11084 = CARTESIAN_POINT ( 'NONE',  ( -0.6156307853269508135, -5.969051238897255196, 5.798705734106810894 ) ) ;
#11085 = EDGE_CURVE ( 'NONE', #14733, #5534, #13526, .T. ) ;
#11086 = CARTESIAN_POINT ( 'NONE',  ( -2.668367453516630849, -5.373994336898132218, 5.000000000000004441 ) ) ;
#11087 = EDGE_CURVE ( 'NONE', #2429, #8910, #5460, .T. ) ;
#11088 = DIRECTION ( 'NONE',  ( 0.8090169943749421222, 0.5877852522924802425, 0.000000000000000000 ) ) ;
#11089 = CARTESIAN_POINT ( 'NONE',  ( -4.267838854167138152, -4.217593933790373839, 11.76239891805595761 ) ) ;
#11090 = DIRECTION ( 'NONE',  ( 0.000000000000000000, 0.000000000000000000, 1.000000000000000000 ) ) ;
#11091 = B_SPLINE_CURVE_WITH_KNOTS ( 'NONE', 3,
 ( #3043, #15374, #4470, #13780, #2887, #7737, #6639, #12666, #497, #5365, #10209, #15062, #7815, #11469, #572, #7896, #9562, #14314 ),
 .UNSPECIFIED., .F., .F.,
 ( 4, 2, 2, 2, 2, 2, 2, 2, 4 ),
 ( 0.000000000000000000, 0.0003914357524127484072, 0.0007828715048254968143, 0.001174307257238245330, 0.001565743009650993629, 0.001957178762063741927, 0.002348614514476490660, 0.002740050266889238959, 0.003131486019301987257 ),
 .UNSPECIFIED. ) ;
#11092 = VECTOR ( 'NONE', #3243, 1000.000000000000000 ) ;
#11093 = CARTESIAN_POINT ( 'NONE',  ( -1.530808498934191571E-16, 2.500000000000000000, 2.299999999999999822 ) ) ;
#11094 = LINE ( 'NONE', #191, #13787 ) ;
#11095 = CARTESIAN_POINT ( 'NONE',  ( 0.000000000000000000, 62.00000000000000000, 0.000000000000000000 ) ) ;
#11096 = CARTESIAN_POINT ( 'NONE',  ( -2.500000000000000444, 185.1199999975965511, 5.964466094067261359 ) ) ;
#11097 = CARTESIAN_POINT ( 'NONE',  ( -1.580027211161896261, 227.8635840621947182, 5.845413847729996171 ) ) ;
#11098 = CARTESIAN_POINT ( 'NONE',  ( 2.990158053860457077, 227.3692281962998436, 7.562228658338257858 ) ) ;
#11099 = CARTESIAN_POINT ( 'NONE',  ( -0.07135113763453279634, 189.0441085615118197, 10.18309864254113073 ) ) ;
#11100 = VERTEX_POINT ( 'NONE', #7381 ) ;
#11101 = CARTESIAN_POINT ( 'NONE',  ( -3.420659742068370424, 4.931142898501745364, 5.999950536462232087 ) ) ;
#11102 = CARTESIAN_POINT ( 'NONE',  ( -6.081464507797602614, 1.446657058464316359, 23.62619944752603374 ) ) ;
#11103 = CARTESIAN_POINT ( 'NONE',  ( -2.692693252389773306, 5.362085866495016617, 24.23617396794404044 ) ) ;
#11104 = CARTESIAN_POINT ( 'NONE',  ( 6.106056299406742660, 1.336851112280702747, 12.29887838423337953 ) ) ;
#11105 = CARTESIAN_POINT ( 'NONE',  ( 2.999999999999999556, -1.732050807568877859, -2.500000000000000000 ) ) ;
#11106 = EDGE_CURVE ( 'NONE', #1290, #13408, #1321, .T. ) ;
#11107 = DIRECTION ( 'NONE',  ( -0.9510565162951545304, 0.3090169943749447867, 0.000000000000000000 ) ) ;
#11108 = CARTESIAN_POINT ( 'NONE',  ( -1.461580736456472795, 1.461580736456472795, -2.649999998907524912 ) ) ;
#11109 = CARTESIAN_POINT ( 'NONE',  ( -2.841519077896339951, 5.566940434249915803, 24.23620383159193636 ) ) ;
#11110 = SURFACE_STYLE_FILL_AREA ( #2279 ) ;
#11111 = CARTESIAN_POINT ( 'NONE',  ( -6.176542424588110869, 0.9554180641286129649, 11.49999999999998224 ) ) ;
#11112 = CARTESIAN_POINT ( 'NONE',  ( -1.767766952966369320, 186.6300000002185016, 5.232233047033630235 ) ) ;
#11113 = DIRECTION ( 'NONE',  ( 0.000000000000000000, 0.000000000000000000, -1.000000000000000000 ) ) ;
#11114 = VECTOR ( 'NONE', #6775, 1000.000000000000000 ) ;
#11115 = CARTESIAN_POINT ( 'NONE',  ( 1.851056454904606685, 228.5003429013454763, 7.684409693542115782 ) ) ;
#11116 = DIRECTION ( 'NONE',  ( 0.000000000000000000, 0.000000000000000000, -1.000000000000000000 ) ) ;
#11117 = CARTESIAN_POINT ( 'NONE',  ( -4.435347140101057128, -4.403429997944487084, 11.49999999999998224 ) ) ;
#11118 = ORIENTED_EDGE ( 'NONE', *, *, #12425, .F. ) ;
#11119 = CARTESIAN_POINT ( 'NONE',  ( -1.461580736456472795, 1.461580736456472795, 0.3500000010924746996 ) ) ;
#11120 = CARTESIAN_POINT ( 'NONE',  ( 2.500000000000000444, 185.5999999999999943, 7.000000000000000000 ) ) ;
#11121 = AXIS2_PLACEMENT_3D ( 'NONE', #10219, #7826, #4244 ) ;
#11123 = ORIENTED_EDGE ( 'NONE', *, *, #12999, .T. ) ;
#11122 = CARTESIAN_POINT ( 'NONE',  ( 2.066987299999999639, 185.9999999989074979, 7.856174172912946396 ) ) ;
#11124 = CARTESIAN_POINT ( 'NONE',  ( 6.780834057763294634E-14, -6.250000000000000888, 10.49999999999998224 ) ) ;
#11125 = AXIS2_PLACEMENT_3D ( 'NONE', #2579, #5506, #4142 ) ;
#11126 = EDGE_CURVE ( 'NONE', #2492, #6851, #5968, .T. ) ;
#11127 = CARTESIAN_POINT ( 'NONE',  ( 5.984377695197257374, -1.807429553002170897, 12.50004906876531052 ) ) ;
#11128 = SURFACE_STYLE_FILL_AREA ( #4858 ) ;
#11129 = CYLINDRICAL_SURFACE ( 'NONE', #9864, 0.9999999999999998890 ) ;
#11130 = CARTESIAN_POINT ( 'NONE',  ( -0.2623718222034516212, -6.245654667075786648, 10.52627829713833485 ) ) ;
#11131 = CARTESIAN_POINT ( 'NONE',  ( 5.903347812666392080, -1.076697810262364552, 25.11397738943081848 ) ) ;
#11132 = CARTESIAN_POINT ( 'NONE',  ( -1.035533905932737753, 2.500000000000000444, -3.149999997815050801 ) ) ;
#11133 = CYLINDRICAL_SURFACE ( 'NONE', #1974, 1.499999999999999556 ) ;
#11134 = CARTESIAN_POINT ( 'NONE',  ( 3.735808404765066371, -4.696639218303072738, 5.973980201222398811 ) ) ;
#11136 = CARTESIAN_POINT ( 'NONE',  ( -5.903119516422478341, 1.077859910107469288, 10.88480617551147134 ) ) ;
#11135 = AXIS2_PLACEMENT_3D ( 'NONE', #2325, #1059, #12037 ) ;
#11137 = DIRECTION ( 'NONE',  ( 0.000000000000000000, 1.000000000000000000, 0.000000000000000000 ) ) ;
#11138 = CARTESIAN_POINT ( 'NONE',  ( -2.500000000000000444, 187.5499999999999829, 5.964466094067261359 ) ) ;
#11139 = ORIENTED_EDGE ( 'NONE', *, *, #12695, .T. ) ;
#11140 = CARTESIAN_POINT ( 'NONE',  ( 2.066987299999999639, 187.5999999989075491, 7.856174172912946396 ) ) ;
#11141 = ORIENTED_EDGE ( 'NONE', *, *, #14453, .F. ) ;
#11142 = EDGE_LOOP ( 'NONE', ( #12330, #3909 ) ) ;
#11143 = CARTESIAN_POINT ( 'NONE',  ( -5.842945980534610229, -1.369128644669114658, 25.37378430870261781 ) ) ;
#11144 = ORIENTED_EDGE ( 'NONE', *, *, #7017, .T. ) ;
#11145 = AXIS2_PLACEMENT_3D ( 'NONE', #7642, #3741, #4872 ) ;
#11146 = CARTESIAN_POINT ( 'NONE',  ( 3.796994071234844259E-16, -2.066987299999999639, 0.6500000010924747995 ) ) ;
#11147 = FACE_OUTER_BOUND ( 'NONE', #8614, .T. ) ;
#11148 = CARTESIAN_POINT ( 'NONE',  ( -0.2771997073367608033, 189.6983012903869223, 10.38340820118765961 ) ) ;
#11149 = CARTESIAN_POINT ( 'NONE',  ( 5.131373506000491247, 7.062729720844170167, 17.99999999999998934 ) ) ;
#11150 = CARTESIAN_POINT ( 'NONE',  ( -1.767766952966368432, -1.767766952966369320, -2.193000000021849694 ) ) ;
#11151 = CARTESIAN_POINT ( 'NONE',  ( -5.903057025253917622, 1.078199533779433450, 31.61561732698606164 ) ) ;
#11152 = ADVANCED_FACE ( 'NONE', ( #5392 ), #8899, .F. ) ;
#11153 = DIRECTION ( 'NONE',  ( -1.000000000000000000, 0.000000000000000000, 0.000000000000000000 ) ) ;
#11154 = CARTESIAN_POINT ( 'NONE',  ( 0.8561741729129463963, -2.066987299999999195, 0.1000000010924748939 ) ) ;
#11155 = CARTESIAN_POINT ( 'NONE',  ( -6.172639027853125349, 0.9816353142770998241, 30.73774718278283302 ) ) ;
#11156 = CARTESIAN_POINT ( 'NONE',  ( -2.191791664054325572, 227.9495085101182781, 9.269582106420829248 ) ) ;
#11157 = EDGE_CURVE ( 'NONE', #5982, #1760, #8983, .T. ) ;
#11158 = ORIENTED_EDGE ( 'NONE', *, *, #2387, .T. ) ;
#11159 = EDGE_LOOP ( 'NONE', ( #11158, #922, #2945, #7240 ) ) ;
#11160 = ORIENTED_EDGE ( 'NONE', *, *, #5363, .F. ) ;
#11162 = CARTESIAN_POINT ( 'NONE',  ( 5.665707375537464507, -1.979196487016696482, 29.99992038825522656 ) ) ;
#11161 = B_SPLINE_CURVE_WITH_KNOTS ( 'NONE', 3,
 ( #3668, #8773, #13604, #4958, #1357, #2479, #3824, #13530, #8621, #8697, #12023, #7185, #1123, #13456, #7339, #4797, #2637, #1279 ),
 .UNSPECIFIED., .F., .F.,
 ( 4, 2, 2, 2, 2, 2, 2, 2, 4 ),
 ( 0.000000000000000000, 0.0003914357524127512261, 0.0007828715048255024522, 0.001174307257238253570, 0.001565743009651004904, 0.001957178762063754504, 0.002348614514476504538, 0.002740050266889254137, 0.003131486019302004171 ),
 .UNSPECIFIED. ) ;
#11163 = CARTESIAN_POINT ( 'NONE',  ( 2.504072367983524394, 189.0000000000000284, 7.091356059880736140 ) ) ;
#11164 = EDGE_LOOP ( 'NONE', ( #8153, #14234, #9425, #10733 ) ) ;
#11165 = CARTESIAN_POINT ( 'NONE',  ( -5.858813228503601422, -2.179803269293405066, 17.02622717124729945 ) ) ;
#11166 = CARTESIAN_POINT ( 'NONE',  ( -2.817313151351126255, -5.579000502529464001, 31.00000000000000000 ) ) ;
#11167 = CARTESIAN_POINT ( 'NONE',  ( 0.1323602877612839734, 6.000000000000000888, 12.49999999999998401 ) ) ;
#11168 = CARTESIAN_POINT ( 'NONE',  ( 1.035533905932738197, 187.7499999978150527, 9.500000000000003553 ) ) ;
#11169 = CARTESIAN_POINT ( 'NONE',  ( -2.500000000000003109, 185.1499999999999773, 5.964466094067263136 ) ) ;
#11170 = CARTESIAN_POINT ( 'NONE',  ( -2.931212650151706622, 5.520239928492792991, 10.99574050496989841 ) ) ;
#11171 = CARTESIAN_POINT ( 'NONE',  ( -3.255128505894417490, 5.336774832660654333, 18.87380055247395205 ) ) ;
#11172 = APPLICATION_PROTOCOL_DEFINITION ( 'draft international standard', 'automotive_design', 1998, #12368 ) ;
#11173 = CARTESIAN_POINT ( 'NONE',  ( 2.500000000000000444, 186.3699999975965511, 7.000000000000000000 ) ) ;
#11174 = CARTESIAN_POINT ( 'NONE',  ( 0.2606415164794526063, 227.6142277459897230, 5.125258584176975774 ) ) ;
#11175 = CARTESIAN_POINT ( 'NONE',  ( -0.6817270424356797198, 226.3498696214933545, 4.559454910794151772 ) ) ;
#11176 = CARTESIAN_POINT ( 'NONE',  ( -2.967000931369979000, 189.2639667020261243, 7.657867365370162993 ) ) ;
#11177 = COLOUR_RGB ( '', 0.66274510, 0.83137255, 0.94901961) ;
#11178 =( GEOMETRIC_REPRESENTATION_CONTEXT ( 3 ) GLOBAL_UNCERTAINTY_ASSIGNED_CONTEXT ( ( #5851 ) ) GLOBAL_UNIT_ASSIGNED_CONTEXT ( ( #6210, #9630, #9863 ) ) REPRESENTATION_CONTEXT ( 'NONE', 'WORKASPACE' ) );
#11179 = EDGE_LOOP ( 'NONE', ( #6230, #11470, #2166, #960 ) ) ;
#11180 = CARTESIAN_POINT ( 'NONE',  ( -5.558508435838167117, 2.857531096718976205, 17.86936067245787285 ) ) ;
#11181 = LINE ( 'NONE', #13561, #13200 ) ;
#11182 = CARTESIAN_POINT ( 'NONE',  ( -3.923477796648708882, 4.541042560386316040, 23.62696220972947359 ) ) ;
#11183 = DIRECTION ( 'NONE',  ( 0.9510565162951500895, 0.3090169943749582204, 0.000000000000000000 ) ) ;
#11184 = CARTESIAN_POINT ( 'NONE',  ( 2.151094780193339773, 227.9624926137814498, 9.307769045389981954 ) ) ;
#11185 = CARTESIAN_POINT ( 'NONE',  ( -2.500000000000000000, 0.000000000000000000, 2.500000000000000000 ) ) ;
#11186 = EDGE_CURVE ( 'NONE', #703, #7333, #4175, .T. ) ;
#11187 = CARTESIAN_POINT ( 'NONE',  ( 0.8561741729129451750, 2.066987299999999639, -1.999999998907525223 ) ) ;
#11188 = CARTESIAN_POINT ( 'NONE',  ( -3.459447313392021162, 5.206669755180872272, 23.52599901976669727 ) ) ;
#11189 = FILL_AREA_STYLE_COLOUR ( '', #3556 ) ;
#11190 = CARTESIAN_POINT ( 'NONE',  ( -4.286401442266675410, -4.198423832313046944, 24.49999999999999289 ) ) ;
#11191 = SHAPE_REPRESENTATION ( 'BR-012', ( #3994, #2026, #7380, #9669, #13721, #6875, #14221, #7627, #10173, #1271, #3303, #760, #4841, #15005, #12196, #11687, #5356, #12953, #6119, #8139, #11616, #2801, #14407, #13909, #6559, #1959, #8843, #5791, #2480, #10861, #7558, #9341, #11369, #15693, #4512, #10610, #10108, #9104, #2220, #11121 ), #8599 ) ;
#11192 = CARTESIAN_POINT ( 'NONE',  ( -1.767766952966369320, 186.7000000000000171, 5.232233047033630235 ) ) ;
#11193 = DIRECTION ( 'NONE',  ( 1.000000000000000000, 0.000000000000000000, 0.000000000000000000 ) ) ;
#11194 = DIRECTION ( 'NONE',  ( 0.5877852522924802425, -0.8090169943749422332, 0.000000000000000000 ) ) ;
#11195 = DIRECTION ( 'NONE',  ( 1.000000000000000000, 0.000000000000000000, 0.000000000000000000 ) ) ;
#11196 = EDGE_CURVE ( 'NONE', #15449, #9005, #317, .T. ) ;
#11197 = CARTESIAN_POINT ( 'NONE',  ( 2.996417732210512330, 5.485687819086936479, 12.11396179408069607 ) ) ;
#11198 = FACE_OUTER_BOUND ( 'NONE', #9746, .T. ) ;
#11199 = CARTESIAN_POINT ( 'NONE',  ( 1.461580736456473240, 189.1499999989075036, 5.538419263543526760 ) ) ;
#11200 = CARTESIAN_POINT ( 'NONE',  ( 1.767766952966369098, 187.1999999978150697, 5.232233047033630235 ) ) ;
#11202 = ORIENTED_EDGE ( 'NONE', *, *, #2807, .F. ) ;
#11201 = CARTESIAN_POINT ( 'NONE',  ( -2.066987300000000527, 188.8499999989074922, 7.000000000000000000 ) ) ;
#11203 = CARTESIAN_POINT ( 'NONE',  ( -1.265664690411614835E-16, 2.066987299999999639, -2.749999998907525001 ) ) ;
#11204 = CARTESIAN_POINT ( 'NONE',  ( 5.131373506000584506, 7.062729720844102665, 31.00000000000000000 ) ) ;
#11205 = CARTESIAN_POINT ( 'NONE',  ( -5.317509234263969375, 2.779225709350972906, 4.869350386511451134 ) ) ;
#11206 = CARTESIAN_POINT ( 'NONE',  ( -0.1323408341374213426, -6.250000000000003553, 12.49999999999998401 ) ) ;
#11207 = CARTESIAN_POINT ( 'NONE',  ( 3.311576095066468106, 5.004818610361379427, 17.02622176056705783 ) ) ;
#11208 = CARTESIAN_POINT ( 'NONE',  ( 2.833833435690741531, 189.2310187018060788, 8.166587331077602485 ) ) ;
#11209 = CARTESIAN_POINT ( 'NONE',  ( 1.767766952966369098, 187.9999999978150527, 5.232233047033630235 ) ) ;
#11210 = CARTESIAN_POINT ( 'NONE',  ( 2.668367453516705012, -5.373994336898094026, 5.130616955321390726 ) ) ;
#11211 = CARTESIAN_POINT ( 'NONE',  ( -2.817313151351206635, 5.579000502529421368, 31.00000000000000000 ) ) ;
#11212 = CARTESIAN_POINT ( 'NONE',  ( -5.317509234263900098, -2.779225709351108797, 11.49999999999998224 ) ) ;
#11213 = CARTESIAN_POINT ( 'NONE',  ( -5.903057025253897194, -1.078199533779561348, 10.88438267301392948 ) ) ;
#11214 = ORIENTED_EDGE ( 'NONE', *, *, #11920, .T. ) ;
#11215 = CARTESIAN_POINT ( 'NONE',  ( 2.066987299999999639, 185.9999999989074979, 7.856174172912946396 ) ) ;
#11216 = B_SPLINE_CURVE_WITH_KNOTS ( 'NONE', 3,
 ( #5810, #5732, #15515, #4380, #4697, #708, #1025, #6932, #6854, #789, #10736, #1980, #8277, #15596, #2132, #14385, #11834, #944 ),
 .UNSPECIFIED., .F., .F.,
 ( 4, 2, 2, 2, 2, 2, 2, 2, 4 ),
 ( 0.000000000000000000, 0.0003914898357794972241, 0.0007829796715589944483, 0.001174469507338491564, 0.001565959343117988897, 0.001957449178897486229, 0.002348939014676983128, 0.002740428850456480461, 0.003131918686235977793 ),
 .UNSPECIFIED. ) ;
#11217 = EDGE_LOOP ( 'NONE', ( #1019, #9403, #2324, #3487 ) ) ;
#11218 = CARTESIAN_POINT ( 'NONE',  ( -5.620879908643893863, -2.102487719022092527, 23.52622176056705783 ) ) ;
#11219 = ORIENTED_EDGE ( 'NONE', *, *, #1528, .T. ) ;
#11220 = PLANE ( 'NONE',  #4793 ) ;
#11221 = LINE ( 'NONE', #12568, #467 ) ;
#11222 = ORIENTED_EDGE ( 'NONE', *, *, #4548, .F. ) ;
#11223 = CARTESIAN_POINT ( 'NONE',  ( -1.265664690411614835E-16, 2.066987299999999639, -0.5499999989075254891 ) ) ;
#11224 = CARTESIAN_POINT ( 'NONE',  ( -4.070863287254132601, 4.743975846881758329, 4.126941084456993813 ) ) ;
#11225 = CARTESIAN_POINT ( 'NONE',  ( -1.101860293008299907, 228.1876483704662633, 9.969866227122023972 ) ) ;
#11226 = DIRECTION ( 'NONE',  ( 0.8090169943749421222, 0.5877852522924802425, 0.000000000000000000 ) ) ;
#11227 = CARTESIAN_POINT ( 'NONE',  ( 2.500000000000000444, 1.035533905932737975, 1.350000000000000089 ) ) ;
#11228 = CARTESIAN_POINT ( 'NONE',  ( 0.000000000000000000, 195.7865323290426716, 12.30567995348059007 ) ) ;
#11229 = ITEM_DEFINED_TRANSFORMATION ( 'NONE', 'NONE', #5791,  #14201 ) ;
#11230 = CARTESIAN_POINT ( 'NONE',  ( 2.782468714962392564, 5.316055268221427710, 5.503897950159861274 ) ) ;
#11231 = CARTESIAN_POINT ( 'NONE',  ( -1.461580736456472795, 1.461580736456472795, -1.049999998907525045 ) ) ;
#11232 = FACE_OUTER_BOUND ( 'NONE', #15477, .T. ) ;
#11233 = CARTESIAN_POINT ( 'NONE',  ( -0.2622538972264072954, 6.245673238944477568, 31.97385994369199125 ) ) ;
#11234 = ORIENTED_EDGE ( 'NONE', *, *, #9620, .F. ) ;
#11235 = VERTEX_POINT ( 'NONE', #2995 ) ;
#11236 = VERTEX_POINT ( 'NONE', #11190 ) ;
#11237 = CARTESIAN_POINT ( 'NONE',  ( 0.5042987395409009865, 5.979983180450066271, 18.87329304179975864 ) ) ;
#11238 = CARTESIAN_POINT ( 'NONE',  ( 2.493490695362371667, 189.0000000000000000, 6.752556055000679791 ) ) ;
#11239 = ORIENTED_EDGE ( 'NONE', *, *, #4466, .F. ) ;
#11240 = CARTESIAN_POINT ( 'NONE',  ( -0.1323602877612193029, -6.000000000000001776, 6.000000000000007105 ) ) ;
#11241 = EDGE_CURVE ( 'NONE', #8921, #15586, #13569, .T. ) ;
#11242 = CARTESIAN_POINT ( 'NONE',  ( 0.6152055445546492640, -5.969096820685154015, 31.79904968670267706 ) ) ;
#11243 = CARTESIAN_POINT ( 'NONE',  ( 0.8738118504726281044, 5.936246475285022584, 12.00357242174242423 ) ) ;
#11244 = CARTESIAN_POINT ( 'NONE',  ( 0.2637975869347971014, 6.245592211692895468, 18.97332839949193684 ) ) ;
#11245 = CARTESIAN_POINT ( 'NONE',  ( 2.500000000000000444, 184.6999999978150697, 7.000000000000000000 ) ) ;
#11246 = CYLINDRICAL_SURFACE ( 'NONE', #12436, 0.9999999999999998890 ) ;
#11247 = AXIS2_PLACEMENT_3D ( 'NONE', #11882, #3455, #10544 ) ;
#11248 = CARTESIAN_POINT ( 'NONE',  ( -5.615811513735041949, 2.743665920700387062, 5.503086438660449886 ) ) ;
#11249 = DIRECTION ( 'NONE',  ( 0.000000000000000000, 0.000000000000000000, -1.000000000000000000 ) ) ;
#11250 = CARTESIAN_POINT ( 'NONE',  ( 9.750000000000003553, 146.0000000000000000, 1.020968533498575461E-13 ) ) ;
#11251 = CARTESIAN_POINT ( 'NONE',  ( -5.421010862427522170E-16, 185.3699999975965511, 9.500000000000001776 ) ) ;
#11252 = CARTESIAN_POINT ( 'NONE',  ( -1.814481855529834764, 227.9916279875985765, 6.215212007442850961 ) ) ;
#11253 = CARTESIAN_POINT ( 'NONE',  ( -2.899241975612990352, 227.5395701600909888, 8.063569561630318461 ) ) ;
#11254 = ADVANCED_FACE ( 'NONE', ( #1477 ), #2842, .F. ) ;
#11255 = CARTESIAN_POINT ( 'NONE',  ( -1.612690174612901650, 189.7356689584554204, 9.916675524984150059 ) ) ;
#11256 = AXIS2_PLACEMENT_3D ( 'NONE', #2623, #5976, #3577 ) ;
#11257 = VERTEX_POINT ( 'NONE', #11345 ) ;
#11258 = CARTESIAN_POINT ( 'NONE',  ( -3.011139120916522138, 5.190534000030338824, 5.799318062581744648 ) ) ;
#11259 = EDGE_CURVE ( 'NONE', #13429, #15355, #10007, .T. ) ;
#11260 = LINE ( 'NONE', #7758, #2532 ) ;
#11261 = CARTESIAN_POINT ( 'NONE',  ( -0.6151877315909838329, 6.220340188096016298, 5.799066734696703307 ) ) ;
#11262 = CARTESIAN_POINT ( 'NONE',  ( 6.155973317223288888, 1.081218830693715161, 12.00308643866043568 ) ) ;
#11263 = CARTESIAN_POINT ( 'NONE',  ( 2.999303574923353644, 227.2680296707977163, 7.264325765249956213 ) ) ;
#11264 = CARTESIAN_POINT ( 'NONE',  ( 3.736691294293340793, -4.695920479336442632, 23.52641404563306082 ) ) ;
#11265 = CARTESIAN_POINT ( 'NONE',  ( -1.035533905932738197, -2.500000000000000000, 1.050000000000000044 ) ) ;
#11266 = CARTESIAN_POINT ( 'NONE',  ( -3.883588957979381640, 4.898466244118830915, 23.52622717124730656 ) ) ;
#11267 = AXIS2_PLACEMENT_3D ( 'NONE', #10215, #9109, #13938 ) ;
#11268 = CARTESIAN_POINT ( 'NONE',  ( -4.344502777243497427, -4.493369211529297580, 30.49610786875029689 ) ) ;
#11269 = CARTESIAN_POINT ( 'NONE',  ( 9.147955830346443662E-17, 185.0000000000000000, 4.500000000000000000 ) ) ;
#11270 = FACE_BOUND ( 'NONE', #13190, .T. ) ;
#11271 = CARTESIAN_POINT ( 'NONE',  ( -1.673363231402341000, 227.9073979391035891, 5.971950823222174520 ) ) ;
#11272 = FACE_OUTER_BOUND ( 'NONE', #5361, .T. ) ;
#11273 = EDGE_CURVE ( 'NONE', #15318, #9802, #7848, .T. ) ;
#11274 = CARTESIAN_POINT ( 'NONE',  ( 5.984377695197293789, -1.807429553002048994, 25.50004906876532473 ) ) ;
#11275 = CARTESIAN_POINT ( 'NONE',  ( -2.066987299999999639, 0.8561741729129455081, 2.000000001092474555 ) ) ;
#11276 = CARTESIAN_POINT ( 'NONE',  ( -2.500000000000000444, 184.4499999999999886, 8.035533905932737753 ) ) ;
#11277 = CARTESIAN_POINT ( 'NONE',  ( -4.267992336621287741, 4.217442018459910180, 18.26194324003146008 ) ) ;
#11279 = EDGE_LOOP ( 'NONE', ( #15102, #3971, #14102, #7624 ) ) ;
#11278 = CARTESIAN_POINT ( 'NONE',  ( 2.066987300000000083, 187.6999999989075150, 6.143825827087054492 ) ) ;
#11280 = CARTESIAN_POINT ( 'NONE',  ( 2.500000000000000000, 188.0000000000000000, 7.000000000000000000 ) ) ;
#11281 = CARTESIAN_POINT ( 'NONE',  ( 0.8499999999999896527, 0.4000000000000097367, -2.619018321873355593 ) ) ;
#11282 = EDGE_CURVE ( 'NONE', #278, #11793, #3264, .T. ) ;
#11283 = SHAPE_REPRESENTATION ( 'finger', ( #14201 ), #4310 ) ;
#11284 = CARTESIAN_POINT ( 'NONE',  ( 0.3133709289737746650, 0.4000000000000062395, -2.571515392583464621 ) ) ;
#11285 = CARTESIAN_POINT ( 'NONE',  ( 3.419318284370122196, 4.932111238568230860, 17.00007997643736957 ) ) ;
#11286 = CARTESIAN_POINT ( 'NONE',  ( 2.278945590441513236, 189.0000000008205916, 8.040059661612891873 ) ) ;
#11287 = CARTESIAN_POINT ( 'NONE',  ( 0.09128442574521389297, -0.3999999999999975797, -2.551849451998178253 ) ) ;
#11288 = CARTESIAN_POINT ( 'NONE',  ( 0.4782965142628293753, 190.0842368319956961, 4.234201933446612109 ) ) ;
#11289 = CARTESIAN_POINT ( 'NONE',  ( -4.006441409774732954, 4.467329318258217441, 30.20111757752059489 ) ) ;
#11290 = CARTESIAN_POINT ( 'NONE',  ( -5.746837578675981995, -1.729433780394334930, 12.49995053646221166 ) ) ;
#11291 = CARTESIAN_POINT ( 'NONE',  ( -1.537640463591734230, 189.0000000000000284, 5.001843613985847092 ) ) ;
#11292 = ORIENTED_EDGE ( 'NONE', *, *, #5722, .F. ) ;
#11293 = CARTESIAN_POINT ( 'NONE',  ( -5.895349312889930360E-16, 187.4499999989075150, 9.066987300000000971 ) ) ;
#11294 = ORIENTED_EDGE ( 'NONE', *, *, #13727, .T. ) ;
#11295 = DIRECTION ( 'NONE',  ( 0.000000000000000000, 0.000000000000000000, 1.000000000000000000 ) ) ;
#11296 = CIRCLE ( 'NONE', #10290, 1.500000000000000000 ) ;
#11297 = B_SPLINE_CURVE_WITH_KNOTS ( 'NONE', 3,
 ( #11398, #10138, #15065, #14907, #14757, #4160, #5290, #8875, #13547, #12277, #11322, #10213, #6329, #6562, #2891, #9030, #186, #500 ),
 .UNSPECIFIED., .F., .F.,
 ( 4, 2, 2, 2, 2, 2, 2, 2, 4 ),
 ( 0.000000000000000000, 0.0003914362731607615316, 0.0007828725463215230633, 0.001174308819482284541, 0.001565745092643046127, 0.001957181365803807496, 0.002348617638964569081, 0.002740053912125330667, 0.003131490185286092253 ),
 .UNSPECIFIED. ) ;
#11298 = ORIENTED_EDGE ( 'NONE', *, *, #5914, .F. ) ;
#11299 = CARTESIAN_POINT ( 'NONE',  ( 0.000000000000000000, 182.0000000000000000, 0.000000000000000000 ) ) ;
#11300 = CARTESIAN_POINT ( 'NONE',  ( 2.500000000000000444, 185.6500000000000057, 5.964466094067262247 ) ) ;
#11301 = ORIENTED_EDGE ( 'NONE', *, *, #10599, .F. ) ;
#11302 = CARTESIAN_POINT ( 'NONE',  ( -0.8561741729129458411, -2.066987299999999195, -1.799999998907525267 ) ) ;
#11303 = CARTESIAN_POINT ( 'NONE',  ( -0.8002302970945222027, 5.947135855825885109, 17.38601773212298696 ) ) ;
#11304 = CARTESIAN_POINT ( 'NONE',  ( -0.8596577831047461649, 189.7079546061267479, 10.26809000054746868 ) ) ;
#11305 = CYLINDRICAL_SURFACE ( 'NONE', #15058, 7.000000000000000000 ) ;
#11306 = CARTESIAN_POINT ( 'NONE',  ( -1.767766952966369098, 1.767766952966369098, -0.7999999999999999334 ) ) ;
#11307 = CLOSED_SHELL ( 'NONE', ( #15667, #8641, #8346, #11564, #12013, #3274, #8389, #15606, #1234, #4149, #4585, #9507, #5125, #6831, #6695, #4346, #3000, #2130, #11669, #14662, #5625, #5449, #12885, #7933, #13685, #2109, #12536, #8033, #5559, #5045, #5691, #7397, #6930, #11436, #4436, #3983, #5718, #7951, #14792, #11761, #8725, #14402, #7175, #1697, #14490, #4883, #10668, #8575, #3661, #11735, #12127, #6394, #2042, #1918, #1409, #1366, #14756, #14704, #5172, #4993, #13585, #1399, #13428, #14548, #395, #4377, #11152, #10894, #3955, #6213, #14695, #12225, #14881, #976, #7280, #5036, #2331, #7606, #13387, #11603, #1555, #8182, #6, #9548, #14052, #4934, #6699, #4637, #11254, #253, #5261, #5434, #5457, #14499, #15118, #13006, #10704, #9204, #9219, #2989, #3024, #4103, #4280, #5656, #4144, #4746 ) ) ;
#11308 = DIRECTION ( 'NONE',  ( 1.000000000000000000, 0.000000000000000000, 0.000000000000000000 ) ) ;
#11309 = CARTESIAN_POINT ( 'NONE',  ( 7.799024015210672900, -1.482594289696959944, 17.99999999999998934 ) ) ;
#11310 = CARTESIAN_POINT ( 'NONE',  ( 1.461580736456473018, -1.461580736456472573, -1.449999998907525178 ) ) ;
#11311 = DIRECTION ( 'NONE',  ( 0.9510565162951500895, 0.3090169943749582204, 0.000000000000000000 ) ) ;
#11312 = CARTESIAN_POINT ( 'NONE',  ( 4.267936573529180322, 4.217499624512267786, 11.76229037835932800 ) ) ;
#11313 = ORIENTED_EDGE ( 'NONE', *, *, #15384, .F. ) ;
#11314 = VERTEX_POINT ( 'NONE', #2103 ) ;
#11315 = ORIENTED_EDGE ( 'NONE', *, *, #1216, .T. ) ;
#11316 = CARTESIAN_POINT ( 'NONE',  ( 0.5031281619709130348, 5.980084330432656969, 17.12602272744524257 ) ) ;
#11317 = CARTESIAN_POINT ( 'NONE',  ( 1.292454556065922411, 189.0000000000001137, 9.144800992884551505 ) ) ;
#11318 = AXIS2_PLACEMENT_3D ( 'NONE', #8174, #10634, #4432 ) ;
#11319 = EDGE_LOOP ( 'NONE', ( #10227, #1662 ) ) ;
#11320 = VECTOR ( 'NONE', #12673, 1000.000000000000000 ) ;
#11321 = CARTESIAN_POINT ( 'NONE',  ( -6.176542424588083335, -0.9554180641287667308, 17.99999999999998934 ) ) ;
#11322 = CARTESIAN_POINT ( 'NONE',  ( 0.9740856415302261428, -6.173834621338571083, 17.73852653055532969 ) ) ;
#11323 = EDGE_CURVE ( 'NONE', #8748, #9879, #13728, .T. ) ;
#11324 = CARTESIAN_POINT ( 'NONE',  ( -2.841041022017402273, 5.567186575787253844, 31.26225281721713145 ) ) ;
#11325 = CARTESIAN_POINT ( 'NONE',  ( 0.6156133477427198075, 6.220296490279940471, 18.79872387345518447 ) ) ;
#11326 = CARTESIAN_POINT ( 'NONE',  ( -2.500000000000000444, 185.0499999978150640, 5.964466094067261359 ) ) ;
#11327 = FACE_OUTER_BOUND ( 'NONE', #7018, .T. ) ;
#11328 = CARTESIAN_POINT ( 'NONE',  ( 5.903230462362969000, 1.077253041748798212, 18.61442521571936837 ) ) ;
#11329 = DIRECTION ( 'NONE',  ( 0.000000000000000000, 1.000000000000000000, 0.000000000000000000 ) ) ;
#11330 = CARTESIAN_POINT ( 'NONE',  ( -2.500000000000000444, 187.6199999975965511, 8.035533905932737753 ) ) ;
#11331 = CARTESIAN_POINT ( 'NONE',  ( -2.710505431213761085E-17, 228.2551366889530016, 10.16828399152529983 ) ) ;
#11332 = CARTESIAN_POINT ( 'NONE',  ( -2.932912173331216898, 227.0860177055994882, 6.728427774621575708 ) ) ;
#11333 = EDGE_CURVE ( 'NONE', #13466, #15372, #1425, .T. ) ;
#11334 = CARTESIAN_POINT ( 'NONE',  ( -2.749342815197933554, 189.8200872727807393, 8.555607185862969644 ) ) ;
#11335 = ORIENTED_EDGE ( 'NONE', *, *, #4948, .F. ) ;
#11336 = CARTESIAN_POINT ( 'NONE',  ( -5.558508435838166228, 2.857531096718976649, 17.99999999999998934 ) ) ;
#11337 = DIRECTION ( 'NONE',  ( -0.000000000000000000, 1.000000000000000000, -0.000000000000000000 ) ) ;
#11338 = CARTESIAN_POINT ( 'NONE',  ( 0.1323736289505031416, -6.249999999999999112, 12.49999999999998579 ) ) ;
#11339 = CARTESIAN_POINT ( 'NONE',  ( 6.021135683317699439, 1.680226122398216226, 12.47377282875266502 ) ) ;
#11340 = CARTESIAN_POINT ( 'NONE',  ( 2.995459646452805380, 227.2354604000217932, 7.168427219998267041 ) ) ;
#11341 = CARTESIAN_POINT ( 'NONE',  ( 2.930922878467498993, 5.520395124723560976, 5.503892131249680908 ) ) ;
#11342 = CARTESIAN_POINT ( 'NONE',  ( -2.500000000000000444, 1.035533905932737753, 2.449999999999999734 ) ) ;
#11343 = CARTESIAN_POINT ( 'NONE',  ( -1.767766952966369765, 188.5000000000000000, 8.767766952966368876 ) ) ;
#11344 =( NAMED_UNIT ( * ) SI_UNIT ( $, .STERADIAN. ) SOLID_ANGLE_UNIT ( ) );
#11345 = CARTESIAN_POINT ( 'NONE',  ( 2.082642335314403343E-14, -6.000000000000000888, 32.00000000000000000 ) ) ;
#11346 = CARTESIAN_POINT ( 'NONE',  ( -1.035533905932737975, 186.6500000000000057, 4.500000000000000888 ) ) ;
#11347 = EDGE_CURVE ( 'NONE', #8051, #12191, #15244, .T. ) ;
#11348 = CARTESIAN_POINT ( 'NONE',  ( -0.8231351400649619121, 227.6668932001845462, 5.277359419731677548 ) ) ;
#11349 = LINE ( 'NONE', #448, #9574 ) ;
#11350 = CARTESIAN_POINT ( 'NONE',  ( 4.435347140100961205, 4.403429997944583008, 11.49999999999998224 ) ) ;
#11351 = CIRCLE ( 'NONE', #14386, 6.000000000000000888 ) ;
#11352 = CARTESIAN_POINT ( 'NONE',  ( -1.461580736456472795, 1.461580736456472795, 1.950000001092474733 ) ) ;
#11353 = CARTESIAN_POINT ( 'NONE',  ( 2.500000000000000444, 184.8499999999999943, 5.964466094067262247 ) ) ;
#11354 = CARTESIAN_POINT ( 'NONE',  ( 6.105747081304200741, -1.338335777572131624, 18.80026515017675592 ) ) ;
#11356 = ORIENTED_EDGE ( 'NONE', *, *, #2610, .F. ) ;
#11355 = CARTESIAN_POINT ( 'NONE',  ( 1.461580736456472795, 189.3499999989074922, 5.538419263543527649 ) ) ;
#11357 = CARTESIAN_POINT ( 'NONE',  ( -4.435347140101107755, -4.403429997944435570, 17.86936067245787996 ) ) ;
#11358 = FACE_OUTER_BOUND ( 'NONE', #9602, .T. ) ;
#11359 = AXIS2_PLACEMENT_3D ( 'NONE', #9224, #1887, #12783 ) ;
#11360 = CARTESIAN_POINT ( 'NONE',  ( 3.659182332138577465E-16, 195.9172377311516016, 6.220370292208427188 ) ) ;
#11361 = CARTESIAN_POINT ( 'NONE',  ( 2.973431353044737602, 189.8579570988357546, 7.753557815461304514 ) ) ;
#11362 = CARTESIAN_POINT ( 'NONE',  ( -5.940390500375766436, 6.474944468551470322, 17.99999999999998934 ) ) ;
#11363 = CARTESIAN_POINT ( 'NONE',  ( 0.3969367148316809146, 189.6994987093958684, 10.36945981054583044 ) ) ;
#11364 = CARTESIAN_POINT ( 'NONE',  ( 5.649053410273073617, -2.675685104943254178, 5.615177803758428787 ) ) ;
#11365 = CARTESIAN_POINT ( 'NONE',  ( 2.000000000000001776, 7.566251093182458196E-16, -2.750000000000003109 ) ) ;
#11366 = LINE ( 'NONE', #314, #3149 ) ;
#11367 = ORIENTED_EDGE ( 'NONE', *, *, #12836, .T. ) ;
#11368 = CARTESIAN_POINT ( 'NONE',  ( -0.8561741729129467293, 186.5999999989075206, 9.066987299999999195 ) ) ;
#11369 = AXIS2_PLACEMENT_3D ( 'NONE', #3923, #9113, #12442 ) ;
#11370 = EDGE_CURVE ( 'NONE', #1119, #8460, #12845, .T. ) ;
#11371 = ORIENTED_EDGE ( 'NONE', *, *, #10776, .F. ) ;
#11372 = DIRECTION ( 'NONE',  ( 1.000000000000000000, -3.326610055774637112E-18, -1.062480551894331163E-17 ) ) ;
#11373 = ORIENTED_EDGE ( 'NONE', *, *, #3786, .F. ) ;
#11374 = PLANE ( 'NONE',  #1495 ) ;
#11375 = CARTESIAN_POINT ( 'NONE',  ( 0.000000000000000000, 184.0000000000000000, 7.000000000000000000 ) ) ;
#11376 = ORIENTED_EDGE ( 'NONE', *, *, #10220, .T. ) ;
#11377 = CARTESIAN_POINT ( 'NONE',  ( 0.8561741729129451750, 2.066987299999999639, -0.5999999989075250895 ) ) ;
#11378 = CARTESIAN_POINT ( 'NONE',  ( -0.6139908388539705442, 5.969238533166628002, 17.19977627912012252 ) ) ;
#11379 = AXIS2_PLACEMENT_3D ( 'NONE', #6084, #3526, #8396 ) ;
#11380 = DIRECTION ( 'NONE',  ( 0.000000000000000000, 0.000000000000000000, 1.000000000000000000 ) ) ;
#11381 = CARTESIAN_POINT ( 'NONE',  ( -2.500000000000000000, 0.000000000000000000, -2.300000000000000266 ) ) ;
#11382 = CARTESIAN_POINT ( 'NONE',  ( 0.2619456584323444082, -5.995505046955608819, 17.02607193928646012 ) ) ;
#11383 = CYLINDRICAL_SURFACE ( 'NONE', #4920, 1.000000000000000000 ) ;
#11384 = CONTEXT_DEPENDENT_SHAPE_REPRESENTATION ( #11872, #1074 ) ;
#11385 = CARTESIAN_POINT ( 'NONE',  ( -2.897581130414634077E-17, 9.750000000000003553, 2.000000000000001776 ) ) ;
#11386 = CARTESIAN_POINT ( 'NONE',  ( -2.066987299999999639, 0.8561741729129452860, -0.1999999989075250117 ) ) ;
#11387 = DIRECTION ( 'NONE',  ( 0.000000000000000000, 0.000000000000000000, -1.000000000000000000 ) ) ;
#11388 = EDGE_LOOP ( 'NONE', ( #13289, #13614, #5342, #1835, #980, #10749, #10588, #11410 ) ) ;
#11389 = ADVANCED_FACE ( 'NONE', ( #5623 ), #10546, .T. ) ;
#11390 = EDGE_LOOP ( 'NONE', ( #8113, #13697 ) ) ;
#11391 = CIRCLE ( 'NONE', #14179, 4.000000000000001776 ) ;
#11392 = ORIENTED_EDGE ( 'NONE', *, *, #15078, .F. ) ;
#11393 = MECHANICAL_DESIGN_GEOMETRIC_PRESENTATION_REPRESENTATION (  '', ( #8367 ), #13683 ) ;
#11394 = CARTESIAN_POINT ( 'NONE',  ( 2.848727059635939973, -5.281416301279907799, 25.11442521571938613 ) ) ;
#11395 = CARTESIAN_POINT ( 'NONE',  ( 2.500000000000000000, 188.6999999978150697, 7.000000000000000000 ) ) ;
#11396 = ORIENTED_EDGE ( 'NONE', *, *, #3699, .F. ) ;
#11397 = CARTESIAN_POINT ( 'NONE',  ( -6.020865209844566301, -1.681180471732242943, 17.02599901976669017 ) ) ;
#11398 = CARTESIAN_POINT ( 'NONE',  ( 1.353717517954364224E-13, -6.250000000000000888, 18.99999999999998934 ) ) ;
#11399 = CARTESIAN_POINT ( 'NONE',  ( -4.416837305303518590, 4.422286678978986529, 31.26190213084010239 ) ) ;
#11400 = CARTESIAN_POINT ( 'NONE',  ( 0.7988860301923814689, 6.199427171881318088, 17.38455580536196265 ) ) ;
#11401 = CARTESIAN_POINT ( 'NONE',  ( 1.035533905932737975, 186.4499999978150697, 4.500000000000000888 ) ) ;
#11402 = FACE_OUTER_BOUND ( 'NONE', #7556, .T. ) ;
#11403 = CARTESIAN_POINT ( 'NONE',  ( -3.567624405365413143, 5.133384272590665098, 18.99995078984292363 ) ) ;
#11404 = CIRCLE ( 'NONE', #3779, 2.000000000000000000 ) ;
#11405 = CARTESIAN_POINT ( 'NONE',  ( 2.500000000000000444, 187.9199999975965625, 8.035533905932739529 ) ) ;
#11406 = CARTESIAN_POINT ( 'NONE',  ( -1.454385272030960907, 228.7057613863525489, 8.277669994545302501 ) ) ;
#11407 = CARTESIAN_POINT ( 'NONE',  ( -2.691043998642291157, 227.7164964219492163, 8.584158233643494285 ) ) ;
#11408 = ORIENTED_EDGE ( 'NONE', *, *, #6498, .T. ) ;
#11409 = CARTESIAN_POINT ( 'NONE',  ( 1.915978517174143692, -1.631420465661153951, -2.500869043012635462 ) ) ;
#11410 = ORIENTED_EDGE ( 'NONE', *, *, #1894, .T. ) ;
#11411 = CARTESIAN_POINT ( 'NONE',  ( 3.158296126777914825, -5.394094919772040697, 5.798878384233398187 ) ) ;
#11412 = CARTESIAN_POINT ( 'NONE',  ( 2.817313151351127587, -5.579000502529462224, 11.49999999999998224 ) ) ;
#11413 = CIRCLE ( 'NONE', #14732, 1.500000000000000000 ) ;
#11414 = CARTESIAN_POINT ( 'NONE',  ( -0.2619041840694833478, 6.245686665308502583, 4.026058494337954485 ) ) ;
#11415 = CARTESIAN_POINT ( 'NONE',  ( 5.858736126997126981, 2.179962889277081040, 30.02640428276699325 ) ) ;
#11416 = CARTESIAN_POINT ( 'NONE',  ( 1.815926964132193566, 228.0606537879605469, 9.596472842544713444 ) ) ;
#11417 = CARTESIAN_POINT ( 'NONE',  ( 4.286401442266448925, -4.198423832313278758, 24.36760611998364467 ) ) ;
#11418 = SURFACE_SIDE_STYLE ('',( #4341 ) ) ;
#11419 = CARTESIAN_POINT ( 'NONE',  ( 1.461580736456472573, 1.461580736456472795, -2.049999998907525267 ) ) ;
#11420 = CARTESIAN_POINT ( 'NONE',  ( 11.25000000000000355, -1.020968533498575335E-13, 2.000000000000001776 ) ) ;
#11421 = SHAPE_REPRESENTATION_RELATIONSHIP ( 'NONE' , 'NONE' ,  #4596, #7656 ) ;
#11422 = CARTESIAN_POINT ( 'NONE',  ( 1.767766952966369098, 188.8999999999999773, 5.232233047033630235 ) ) ;
#11423 = CARTESIAN_POINT ( 'NONE',  ( 1.767766952966368654, 184.7000000000000171, 8.767766952966368876 ) ) ;
#11425 = CARTESIAN_POINT ( 'NONE',  ( 1.620240533814224060, 227.8813442971431016, 5.896706419237646379 ) ) ;
#11424 = PRESENTATION_LAYER_ASSIGNMENT (  '', '', ( #13213 ) ) ;
#11426 = DIRECTION ( 'NONE',  ( 0.000000000000000000, 0.000000000000000000, 1.000000000000000000 ) ) ;
#11427 = CARTESIAN_POINT ( 'NONE',  ( 2.840966774240165194, 5.567223638426907151, 11.76190213084010239 ) ) ;
#11428 = CARTESIAN_POINT ( 'NONE',  ( 2.066987299999999639, 0.8561741729129456191, -2.299999998907525711 ) ) ;
#11429 = CARTESIAN_POINT ( 'NONE',  ( -1.767766952966369098, 185.0999999999999943, 5.232233047033630235 ) ) ;
#11430 = CARTESIAN_POINT ( 'NONE',  ( 6.176542424588141955, -0.9554180641284083508, 18.13063932754212004 ) ) ;
#11432 = VERTEX_POINT ( 'NONE', #4500 ) ;
#11431 = CARTESIAN_POINT ( 'NONE',  ( -6.877907531704918753E-16, 189.0499999989075093, 9.066987300000000971 ) ) ;
#11433 = CARTESIAN_POINT ( 'NONE',  ( -2.668367453516752974, -5.373994336898072710, 17.99999999999998934 ) ) ;
#11434 = EDGE_CURVE ( 'NONE', #1738, #8762, #10886, .T. ) ;
#11435 = CARTESIAN_POINT ( 'NONE',  ( 5.935543223013879377, -0.8771126767605279539, 17.99999999999998934 ) ) ;
#11436 = ADVANCED_FACE ( 'NONE', ( #4584 ), #5778, .F. ) ;
#11437 = CARTESIAN_POINT ( 'NONE',  ( 0.000000000000000000, 194.5935680195190116, 12.11154058223188201 ) ) ;
#11438 = CARTESIAN_POINT ( 'NONE',  ( 2.504072369575190748, 189.0000000010835208, 7.091356059128075096 ) ) ;
#11439 = CARTESIAN_POINT ( 'NONE',  ( 4.322356511625485176, 7.650514973136679941, 24.49999999999999289 ) ) ;
#11440 = CARTESIAN_POINT ( 'NONE',  ( -5.935543223013847403, -0.8771126767607488883, 5.132393880016354437 ) ) ;
#11441 = CARTESIAN_POINT ( 'NONE',  ( 3.633127580202335505, -4.776802569231014317, 6.000079611744768115 ) ) ;
#11442 = CARTESIAN_POINT ( 'NONE',  ( 6.176542424588118863, -0.9554180641285446862, 5.000000000000004441 ) ) ;
#11443 = CARTESIAN_POINT ( 'NONE',  ( -5.940390500375711369, 6.474944468551510290, 11.49999999999998224 ) ) ;
#11444 = CARTESIAN_POINT ( 'NONE',  ( 9.750000000000003553, 19.99999999999999645, 1.020968533498575335E-13 ) ) ;
#11445 = ORIENTED_EDGE ( 'NONE', *, *, #8740, .T. ) ;
#11446 = CARTESIAN_POINT ( 'NONE',  ( 1.461580736456472351, 188.3499999989074922, 8.461580736456474128 ) ) ;
#11447 = ORIENTED_EDGE ( 'NONE', *, *, #5811, .T. ) ;
#11448 = CARTESIAN_POINT ( 'NONE',  ( -5.866923913994616768, 1.260079467906669137, 25.29952054102715664 ) ) ;
#11449 = ORIENTED_EDGE ( 'NONE', *, *, #9889, .F. ) ;
#11450 = DIRECTION ( 'NONE',  ( 0.000000000000000000, 0.000000000000000000, 1.000000000000000000 ) ) ;
#11451 = CARTESIAN_POINT ( 'NONE',  ( -2.500000000000000444, 186.0000000000000000, 7.000000000000000000 ) ) ;
#11452 = B_SPLINE_CURVE_WITH_KNOTS ( 'NONE', 3,
 ( #1995, #10286, #14085, #8053, #6869, #13932 ),
 .UNSPECIFIED., .F., .F.,
 ( 4, 2, 4 ),
 ( 0.05507452630550478678, 0.5261283886372931651, 0.9743590206738933501 ),
 .UNSPECIFIED. ) ;
#11453 = ORIENTED_EDGE ( 'NONE', *, *, #13975, .F. ) ;
#11454 = CARTESIAN_POINT ( 'NONE',  ( -2.066987299999999639, 0.000000000000000000, -2.749999998907525445 ) ) ;
#11455 = CARTESIAN_POINT ( 'NONE',  ( -0.7993282387949770529, 5.947240459526529577, 18.61484358216956991 ) ) ;
#11456 = CARTESIAN_POINT ( 'NONE',  ( -4.070863287254068652, -4.743975846881813396, 5.873058915543009739 ) ) ;
#11457 = CARTESIAN_POINT ( 'NONE',  ( 2.500000000000000000, 3.061616997868383141E-16, -0.2999999999999999334 ) ) ;
#11458 = CARTESIAN_POINT ( 'NONE',  ( -6.105925084677690684, -1.337450587213149467, 5.799331489075775004 ) ) ;
#11459 = FACE_BOUND ( 'NONE', #3175, .T. ) ;
#11460 = CONTEXT_DEPENDENT_SHAPE_REPRESENTATION ( #11671, #13400 ) ;
#11461 = CARTESIAN_POINT ( 'NONE',  ( 1.035533905932738197, 187.0499999999999829, 9.500000000000000000 ) ) ;
#11462 = B_SPLINE_CURVE_WITH_KNOTS ( 'NONE', 3,
 ( #12479, #387, #2704, #5257, #12559, #1657, #13753 ),
 .UNSPECIFIED., .F., .F.,
 ( 4, 3, 4 ),
 ( 0.004471049636503268004, 0.004805482912052319762, 0.005232732616948215093 ),
 .UNSPECIFIED. ) ;
#11463 = CARTESIAN_POINT ( 'NONE',  ( -1.461580736456472795, 1.461580736456472795, -1.849999998907525534 ) ) ;
#11464 = DIRECTION ( 'NONE',  ( 0.000000000000000000, 1.000000000000000000, 0.000000000000000000 ) ) ;
#11465 = ORIENTED_EDGE ( 'NONE', *, *, #13089, .T. ) ;
#11466 = ORIENTED_EDGE ( 'NONE', *, *, #11347, .F. ) ;
#11467 = EDGE_LOOP ( 'NONE', ( #8477, #144 ) ) ;
#11468 = CARTESIAN_POINT ( 'NONE',  ( 4.435347140101025154, -4.403429997944519059, 11.49999999999998224 ) ) ;
#11469 = CARTESIAN_POINT ( 'NONE',  ( 6.143143148203035864, 1.154591847827815654, 4.386038205919295940 ) ) ;
#11470 = ORIENTED_EDGE ( 'NONE', *, *, #4720, .F. ) ;
#11471 = CARTESIAN_POINT ( 'NONE',  ( 1.035533905932739085, -2.500000000000000000, -0.3499999978150503677 ) ) ;
#11472 = CARTESIAN_POINT ( 'NONE',  ( -0.8002720181889466655, 6.199262377003425861, 17.38606262465554053 ) ) ;
#11473 = CARTESIAN_POINT ( 'NONE',  ( -6.176542424588083335, -0.9554180641287667308, 17.99999999999998934 ) ) ;
#11474 = CARTESIAN_POINT ( 'NONE',  ( -4.743384504624081899E-17, 187.2999999978150356, 4.500000000000000000 ) ) ;
#11475 = EDGE_CURVE ( 'NONE', #3143, #3208, #2907, .T. ) ;
#11476 = DIRECTION ( 'NONE',  ( -0.000000000000000000, 1.000000000000000000, -0.000000000000000000 ) ) ;
#11477 = CARTESIAN_POINT ( 'NONE',  ( 2.668367453516568677, 5.373994336898162416, 11.49999999999998224 ) ) ;
#11478 = DIRECTION ( 'NONE',  ( 6.982962677686266711E-15, 0.000000000000000000, -1.000000000000000000 ) ) ;
#11479 = VECTOR ( 'NONE', #9826, 1000.000000000000114 ) ;
#11480 = CARTESIAN_POINT ( 'NONE',  ( 1.035533905932738197, 188.6199999975965511, 9.500000000000003553 ) ) ;
#11481 = CARTESIAN_POINT ( 'NONE',  ( 2.349311747835623354, 227.8901172732836642, 9.094898149752092209 ) ) ;
#11482 = EDGE_CURVE ( 'NONE', #14655, #7182, #6981, .T. ) ;
#11483 = CARTESIAN_POINT ( 'NONE',  ( -2.923025936753522291, 227.5090509392885281, 7.973756422523831766 ) ) ;
#11484 = EDGE_LOOP ( 'NONE', ( #13124, #2069, #12503, #3326 ) ) ;
#11485 = CARTESIAN_POINT ( 'NONE',  ( 3.107278289587274589, -5.134157760521997460, 4.126352953155772774 ) ) ;
#11486 = ORIENTED_EDGE ( 'NONE', *, *, #2984, .F. ) ;
#11487 = CARTESIAN_POINT ( 'NONE',  ( -2.817313151351311884, 5.579000502529370742, 17.99999999999998934 ) ) ;
#11488 = CARTESIAN_POINT ( 'NONE',  ( 2.500000000000000000, 189.4499999978150697, 8.035533905932739529 ) ) ;
#11489 = LINE ( 'NONE', #13954, #1173 ) ;
#11490 = DIRECTION ( 'NONE',  ( 0.000000000000000000, 0.000000000000000000, 1.000000000000000000 ) ) ;
#11491 = CIRCLE ( 'NONE', #4640, 1.999999999999999556 ) ;
#11492 = DIRECTION ( 'NONE',  ( -0.9510565162951545304, 0.3090169943749447867, 0.000000000000000000 ) ) ;
#11493 = DIRECTION ( 'NONE',  ( 0.000000000000000000, 0.000000000000000000, -1.000000000000000000 ) ) ;
#11494 = CARTESIAN_POINT ( 'NONE',  ( 4.435347140100977192, -4.403429997944567020, 17.99999999999998934 ) ) ;
#11495 = CARTESIAN_POINT ( 'NONE',  ( -1.035533905932738197, -2.500000000000000000, -0.5500000000000001554 ) ) ;
#11496 = CARTESIAN_POINT ( 'NONE',  ( 0.000000000000000000, 184.0000000000000000, -7.000000000000000000 ) ) ;
#11497 = CARTESIAN_POINT ( 'NONE',  ( 5.867109477881220059, 1.259218163101030186, 5.798882422479413101 ) ) ;
#11498 = CARTESIAN_POINT ( 'NONE',  ( 2.500000000000000444, 185.6500000000000341, 5.964466094067262247 ) ) ;
#11499 = CARTESIAN_POINT ( 'NONE',  ( 1.725625307041983136, 227.9349420198840903, 6.051499699527947307 ) ) ;
#11500 = PRODUCT_DEFINITION_CONTEXT ( 'detailed design', #13184, 'design' ) ;
#11501 = CARTESIAN_POINT ( 'NONE',  ( 0.000000000000000000, 0.000000000000000000, 36.00000000000000711 ) ) ;
#11502 = CIRCLE ( 'NONE', #6693, 1.499999999999999556 ) ;
#11503 = CARTESIAN_POINT ( 'NONE',  ( 6.176542424588121527, -0.9554180641285241471, 30.86939309276501575 ) ) ;
#11504 = CARTESIAN_POINT ( 'NONE',  ( 1.461580736456472573, 1.461580736456472795, -1.449999998907525178 ) ) ;
#11505 = CARTESIAN_POINT ( 'NONE',  ( -6.911788849595090767E-16, 187.7999999999999829, 9.500000000000001776 ) ) ;
#11506 = CARTESIAN_POINT ( 'NONE',  ( 4.435347140100929231, -4.403429997944614982, 24.63234125634167526 ) ) ;
#11508 = ORIENTED_EDGE ( 'NONE', *, *, #14007, .F. ) ;
#11507 = CARTESIAN_POINT ( 'NONE',  ( -0.8561741729129469514, 187.3999999989075889, 9.066987299999999195 ) ) ;
#11509 = CARTESIAN_POINT ( 'NONE',  ( -2.817313151351230172, -5.579000502529412486, 17.99999999999998934 ) ) ;
#11510 = CARTESIAN_POINT ( 'NONE',  ( 2.692143549875217978, 5.362363179736568952, 24.76194324003146008 ) ) ;
#11511 = EDGE_CURVE ( 'NONE', #12347, #920, #14117, .T. ) ;
#11512 = CARTESIAN_POINT ( 'NONE',  ( -5.903119516422490776, 1.077859910107415331, 4.384806175511481996 ) ) ;
#11513 = DIRECTION ( 'NONE',  ( 0.000000000000000000, 0.000000000000000000, 1.000000000000000000 ) ) ;
#11514 = CARTESIAN_POINT ( 'NONE',  ( 2.046085423705328310, 189.0000000012578028, 8.444739455527990657 ) ) ;
#11515 = CARTESIAN_POINT ( 'NONE',  ( 2.082642335314403343E-14, -6.250000000000000888, 32.00000000000000000 ) ) ;
#11516 = CARTESIAN_POINT ( 'NONE',  ( -5.375763363753442547, -2.665284979407549049, 5.503897950159861274 ) ) ;
#11517 = CARTESIAN_POINT ( 'NONE',  ( 1.964981070171530675, 228.3669111765908895, 7.299051262003229290 ) ) ;
#11518 = CARTESIAN_POINT ( 'NONE',  ( 5.770288754215199489, -2.404361317819788901, 23.62618035954928786 ) ) ;
#11519 = CARTESIAN_POINT ( 'NONE',  ( -6.105925084677707559, 1.337450587213069753, 4.200668510924230326 ) ) ;
#11520 = CARTESIAN_POINT ( 'NONE',  ( -5.842988226680550845, -1.369004370660760861, 10.62619317285287934 ) ) ;
#11521 = EDGE_LOOP ( 'NONE', ( #7336, #12954 ) ) ;
#11522 = CARTESIAN_POINT ( 'NONE',  ( -2.066987300000000971, 186.1999999989075150, 6.143825827087054492 ) ) ;
#11523 = AXIS2_PLACEMENT_3D ( 'NONE', #4634, #4474, #9328 ) ;
#11524 = EDGE_CURVE ( 'NONE', #11793, #2012, #14744, .T. ) ;
#11525 = ORIENTED_EDGE ( 'NONE', *, *, #13524, .F. ) ;
#11526 = CARTESIAN_POINT ( 'NONE',  ( 4.286401442266518202, 4.198423832313208592, 31.00000000000000000 ) ) ;
#11527 = ORIENTED_EDGE ( 'NONE', *, *, #13420, .T. ) ;
#11528 = FACE_OUTER_BOUND ( 'NONE', #8577, .T. ) ;
#11529 = CARTESIAN_POINT ( 'NONE',  ( -5.330004929009570347, -2.755647751839434445, 30.73760108194403173 ) ) ;
#11530 = CARTESIAN_POINT ( 'NONE',  ( -1.084202172485504434E-15, -3.464101615137755275, -5.500000000000000000 ) ) ;
#11531 = CARTESIAN_POINT ( 'NONE',  ( 5.867109477881279567, -1.259218163100750854, 23.70111757752058068 ) ) ;
#11532 = CARTESIAN_POINT ( 'NONE',  ( -1.530808498934191571E-16, 2.500000000000000000, -1.700000000000000622 ) ) ;
#11533 = CARTESIAN_POINT ( 'NONE',  ( 0.5039079366033875074, -5.980031194523140137, 17.12637068109812333 ) ) ;
#11534 = CARTESIAN_POINT ( 'NONE',  ( -0.001074311305641557088, 226.3251817249170017, 4.486671161788877704 ) ) ;
#11535 = CARTESIAN_POINT ( 'NONE',  ( 1.767766952966368432, 187.0999999999999943, 8.767766952966368876 ) ) ;
#11536 = CARTESIAN_POINT ( 'NONE',  ( -5.915641100987802048, -1.003868594704925510, 17.49571079637980020 ) ) ;
#11537 = CARTESIAN_POINT ( 'NONE',  ( -1.767766952966369320, 186.5999999978150754, 5.232233047033630235 ) ) ;
#11538 = AXIS2_PLACEMENT_3D ( 'NONE', #5471, #4023, #10239 ) ;
#11539 = EDGE_CURVE ( 'NONE', #12035, #727, #817, .T. ) ;
#11540 = ORIENTED_EDGE ( 'NONE', *, *, #7368, .T. ) ;
#11541 = ORIENTED_EDGE ( 'NONE', *, *, #12054, .F. ) ;
#11542 = ORIENTED_EDGE ( 'NONE', *, *, #13770, .T. ) ;
#11543 = CARTESIAN_POINT ( 'NONE',  ( 2.782156709077311163, -5.316215864844103578, 25.00312048902378237 ) ) ;
#11544 = DIRECTION ( 'NONE',  ( -1.000000000000000000, 0.000000000000000000, 0.000000000000000000 ) ) ;
#11545 = ADVANCED_FACE ( 'NONE', ( #11074, #6316 ), #1521, .F. ) ;
#11546 = VERTEX_POINT ( 'NONE', #7574 ) ;
#11547 = CARTESIAN_POINT ( 'NONE',  ( 5.531796221294931648, -2.326749136277085128, 18.87378430870261781 ) ) ;
#11548 = B_SPLINE_CURVE_WITH_KNOTS ( 'NONE', 3,
 ( #15479, #13240, #11878, #4279, #1066, #11801, #15718, #4737, #9144, #5930, #1803, #10777, #5852, #15635, #8317, #15557, #2173, #4657 ),
 .UNSPECIFIED., .F., .F.,
 ( 4, 2, 2, 2, 2, 2, 2, 2, 4 ),
 ( 0.003131490185286087483, 0.003522829482338687979, 0.003914168779391288475, 0.004305508076443888971, 0.004696847373496489467, 0.005088186670549089963, 0.005479525967601690459, 0.005870865264654290955, 0.006262204561706891451 ),
 .UNSPECIFIED. ) ;
#11549 = CARTESIAN_POINT ( 'NONE',  ( -1.767766952966368432, -1.767766952966369320, 0.3000000021849495990 ) ) ;
#11550 = AXIS2_PLACEMENT_3D ( 'NONE', #7273, #15703, #3678 ) ;
#11551 = CARTESIAN_POINT ( 'NONE',  ( -9.750000000000003553, 3.401296724241641415E-14, 2.000000000000001776 ) ) ;
#11552 = CARTESIAN_POINT ( 'NONE',  ( 3.254737477227823472, 5.337033878705316425, 25.37367328635992081 ) ) ;
#11553 = CARTESIAN_POINT ( 'NONE',  ( 8.809142651444723526E-17, 184.6499999989075320, 4.933012699999999029 ) ) ;
#11554 = DIRECTION ( 'NONE',  ( -1.000000000000000000, 3.326610055774637112E-18, 1.062480551894331163E-17 ) ) ;
#11555 = EDGE_CURVE ( 'NONE', #5302, #4447, #5198, .T. ) ;
#11556 = DIRECTION ( 'NONE',  ( 1.000000000000000000, 0.000000000000000000, 0.000000000000000000 ) ) ;
#11557 = CARTESIAN_POINT ( 'NONE',  ( -2.500000000000000000, 0.000000000000000000, -0.7000000000000000666 ) ) ;
#11558 = CARTESIAN_POINT ( 'NONE',  ( 1.767766952966368432, 189.4699999975965738, 8.767766952966368876 ) ) ;
#11559 = CARTESIAN_POINT ( 'NONE',  ( 0.6804430692981219275, 228.2300923459994237, 10.09465452691961751 ) ) ;
#11560 = CYLINDRICAL_SURFACE ( 'NONE', #2666, 0.9999999999999998890 ) ;
#11561 = ORIENTED_EDGE ( 'NONE', *, *, #9159, .F. ) ;
#11562 = CLOSED_SHELL ( 'NONE', ( #6729, #7626, #7693, #5143, #10187, #12316, #7313, #15388, #729, #2408, #7462, #15056, #15229, #6736, #10665, #6560, #15232, #8491, #838, #15001, #10575, #5759, #5377, #14754, #5223, #2702, #4546, #15467, #10959, #3592, #958 ) ) ;
#11563 = CARTESIAN_POINT ( 'NONE',  ( 0.02052235255247245385, -2.503876325069105402, -2.499973232076210472 ) ) ;
#11564 = ADVANCED_FACE ( 'NONE', ( #20 ), #9891, .F. ) ;
#11565 = ORIENTED_EDGE ( 'NONE', *, *, #13222, .F. ) ;
#11566 = CARTESIAN_POINT ( 'NONE',  ( 0.8499999999999896527, 0.4000000000000062395, 2.619018321873338273 ) ) ;
#11567 = DIRECTION ( 'NONE',  ( 0.8660254037844385966, 0.4999999999999998890, 0.000000000000000000 ) ) ;
#11568 = CARTESIAN_POINT ( 'NONE',  ( 5.984377695197266256, 1.807429553002144917, 23.49995093123466461 ) ) ;
#11569 = CARTESIAN_POINT ( 'NONE',  ( -5.329907877631334223, 2.755840666746301348, 17.73805675996853637 ) ) ;
#11570 = FACE_BOUND ( 'NONE', #14731, .T. ) ;
#11571 = CARTESIAN_POINT ( 'NONE',  ( 6.105747081304183865, -1.338335777572222440, 31.80026515017675592 ) ) ;
#11572 = VECTOR ( 'NONE', #9523, 1000.000000000000114 ) ;
#11573 = CARTESIAN_POINT ( 'NONE',  ( 1.035533905932739085, -2.500000000000000000, 0.3500000000000000333 ) ) ;
#11574 = CARTESIAN_POINT ( 'NONE',  ( 1.035533905932738197, 188.6499999999999773, 9.500000000000000000 ) ) ;
#11575 =( NAMED_UNIT ( * ) PLANE_ANGLE_UNIT ( ) SI_UNIT ( $, .RADIAN. ) );
#11576 = CARTESIAN_POINT ( 'NONE',  ( -2.500000000000000444, 1.035533905932737753, 1.750000002184949999 ) ) ;
#11577 = CARTESIAN_POINT ( 'NONE',  ( 2.500000000000000444, 186.2999999978150356, 7.000000000000000000 ) ) ;
#11578 =( REPRESENTATION_RELATIONSHIP ('NONE','NONE', #11191, #3660 ) REPRESENTATION_RELATIONSHIP_WITH_TRANSFORMATION ( #13225 )SHAPE_REPRESENTATION_RELATIONSHIP( ) );
#11579 = CARTESIAN_POINT ( 'NONE',  ( -1.990672364496464342, 228.2390692824501457, 6.929836580100483090 ) ) ;
#11580 = DIRECTION ( 'NONE',  ( 0.000000000000000000, 0.000000000000000000, 1.000000000000000000 ) ) ;
#11581 = CARTESIAN_POINT ( 'NONE',  ( 0.9999171162591851125, 6.169494774098513545, 24.36722320330680347 ) ) ;
#11582 = CARTESIAN_POINT ( 'NONE',  ( 2.066987300000000083, -0.8561741729129450640, -2.399999998907525356 ) ) ;
#11583 = CARTESIAN_POINT ( 'NONE',  ( 2.500000000000000000, 188.7999999999999829, 7.000000000000000000 ) ) ;
#11584 = CARTESIAN_POINT ( 'NONE',  ( -2.817313151351373168, 5.579000502529340544, 24.63237410716306286 ) ) ;
#11585 = EDGE_CURVE ( 'NONE', #8963, #12601, #8036, .T. ) ;
#11587 = EDGE_LOOP ( 'NONE', ( #4646, #9524, #13542, #11915 ) ) ;
#11586 = CARTESIAN_POINT ( 'NONE',  ( 2.030576276931546336E-13, -6.000000000000000888, 25.49999999999999645 ) ) ;
#11588 = DIRECTION ( 'NONE',  ( 0.8090169943749506709, -0.5877852522924689183, 0.000000000000000000 ) ) ;
#11589 = CARTESIAN_POINT ( 'NONE',  ( -1.461580736456472795, 1.461580736456472795, 2.150000001092474911 ) ) ;
#11590 = CARTESIAN_POINT ( 'NONE',  ( -1.579607963155742922, 189.7340877847497325, 9.937618139430700381 ) ) ;
#11591 = CARTESIAN_POINT ( 'NONE',  ( 0.9527618732035531002, 189.4347749068571432, 4.132041495851004775 ) ) ;
#11592 = CARTESIAN_POINT ( 'NONE',  ( 2.500000000000000444, 184.6800000002185129, 8.035533905932739529 ) ) ;
#11593 = CARTESIAN_POINT ( 'NONE',  ( -0.1323933160975409862, 6.000000000000000000, 32.00000000000000000 ) ) ;
#11594 = VECTOR ( 'NONE', #14958, 1000.000000000000114 ) ;
#11595 = CARTESIAN_POINT ( 'NONE',  ( 1.990661649217015494, 228.2715988311494471, 7.023783772108481038 ) ) ;
#11596 = CARTESIAN_POINT ( 'NONE',  ( 2.066987300000000527, 184.2499999989074979, 7.000000000000000000 ) ) ;
#11597 = CARTESIAN_POINT ( 'NONE',  ( -6.172639027853131566, 0.9816353142770681828, 4.737747182782872990 ) ) ;
#11598 = CARTESIAN_POINT ( 'NONE',  ( -2.668367453516648169, -5.373994336898123336, 31.00000000000000000 ) ) ;
#11599 = ORIENTED_EDGE ( 'NONE', *, *, #13970, .T. ) ;
#11600 = CARTESIAN_POINT ( 'NONE',  ( -4.811147140404425926E-16, 185.6499999989075320, 9.066987300000000971 ) ) ;
#11601 = PRODUCT_DEFINITION_SHAPE ( 'NONE', 'NONE',  #15753 ) ;
#11602 = CARTESIAN_POINT ( 'NONE',  ( 6.780834062235653815E-14, 6.000000000000000888, 10.49999999999998224 ) ) ;
#11603 = ADVANCED_FACE ( 'NONE', ( #15131 ), #4306, .F. ) ;
#11604 = ORIENTED_EDGE ( 'NONE', *, *, #15038, .T. ) ;
#11605 = FACE_BOUND ( 'NONE', #11869, .T. ) ;
#11606 = CYLINDRICAL_SURFACE ( 'NONE', #6349, 1.000000000000000666 ) ;
#11607 = VECTOR ( 'NONE', #2199, 1000.000000000000000 ) ;
#11608 = CARTESIAN_POINT ( 'NONE',  ( -5.620879908643956924, -2.102487719021920221, 30.02622176056706138 ) ) ;
#11609 = LINE ( 'NONE', #5654, #12142 ) ;
#11610 = CARTESIAN_POINT ( 'NONE',  ( 3.253823204785017964, 5.337590213880564427, 17.12694108445698404 ) ) ;
#11611 = CARTESIAN_POINT ( 'NONE',  ( -1.461580736456473018, 184.5499999989075093, 5.538419263543526760 ) ) ;
#11612 = CARTESIAN_POINT ( 'NONE',  ( 7.490007020835686369, -2.433650805992243260, 5.000000000000004441 ) ) ;
#11613 = CARTESIAN_POINT ( 'NONE',  ( -2.500000000000000000, -1.035533905932739307, -1.450000000000000400 ) ) ;
#11614 = DIRECTION ( 'NONE',  ( 0.000000000000000000, 1.000000000000000000, 0.000000000000000000 ) ) ;
#11615 = CARTESIAN_POINT ( 'NONE',  ( 5.999999999999999112, 215.0542865858234336, 7.296348638370669271 ) ) ;
#11617 = CARTESIAN_POINT ( 'NONE',  ( 2.500000000000000444, 187.1499999999999773, 8.035533905932739529 ) ) ;
#11616 = AXIS2_PLACEMENT_3D ( 'NONE', #9591, #1228, #15640 ) ;
#11618 = FACE_OUTER_BOUND ( 'NONE', #6999, .T. ) ;
#11619 = CYLINDRICAL_SURFACE ( 'NONE', #4404, 1.000000000000000888 ) ;
#11620 = VECTOR ( 'NONE', #8993, 1000.000000000000000 ) ;
#11621 = EDGE_LOOP ( 'NONE', ( #12348, #15192 ) ) ;
#11622 = ORIENTED_EDGE ( 'NONE', *, *, #2090, .F. ) ;
#11623 = ORIENTED_EDGE ( 'NONE', *, *, #8439, .T. ) ;
#11624 = CARTESIAN_POINT ( 'NONE',  ( 3.780072143464169976, -4.979057943639785933, 19.00008219321555814 ) ) ;
#11625 = CYLINDRICAL_SURFACE ( 'NONE', #12400, 1.000000000000000000 ) ;
#11626 = ORIENTED_EDGE ( 'NONE', *, *, #11524, .F. ) ;
#11627 = AXIS2_PLACEMENT_3D ( 'NONE', #14070, #15358, #7958 ) ;
#11628 = CARTESIAN_POINT ( 'NONE',  ( 2.500000000000000000, 3.061616997868383141E-16, -0.1999999978150504010 ) ) ;
#11629 = AXIS2_PLACEMENT_3D ( 'NONE', #11695, #795, #5661 ) ;
#11630 = EDGE_CURVE ( 'NONE', #14401, #14543, #14080, .T. ) ;
#11631 = CARTESIAN_POINT ( 'NONE',  ( -0.8737888311108027439, 5.936248257219539859, 25.00344185141216613 ) ) ;
#11632 = CARTESIAN_POINT ( 'NONE',  ( 2.840966774240040404, 5.567223638426967547, 24.76190213084013081 ) ) ;
#11633 = CARTESIAN_POINT ( 'NONE',  ( -1.767766952966369765, 188.3999999978150584, 8.767766952966368876 ) ) ;
#11634 = DIRECTION ( 'NONE',  ( 0.5877852522924802425, -0.8090169943749422332, 0.000000000000000000 ) ) ;
#11635 = EDGE_CURVE ( 'NONE', #3215, #7968, #3188, .T. ) ;
#11636 = CARTESIAN_POINT ( 'NONE',  ( -2.500000000000000444, 185.8499999978150754, 5.964466094067261359 ) ) ;
#11637 = CARTESIAN_POINT ( 'NONE',  ( 0.8561741729129463963, -2.066987299999999195, 0.7000000010924749549 ) ) ;
#11638 = CARTESIAN_POINT ( 'NONE',  ( -5.409007216690671527, -2.598315788643751123, 4.385574784280630745 ) ) ;
#11639 = CARTESIAN_POINT ( 'NONE',  ( -0.1300625424525254092, 228.9108363453237303, 8.869938172763147222 ) ) ;
#11640 = CARTESIAN_POINT ( 'NONE',  ( -2.500000000000000000, 0.000000000000000000, 1.000000002184949777 ) ) ;
#11641 = AXIS2_PLACEMENT_3D ( 'NONE', #14885, #6229, #3972 ) ;
#11642 = EDGE_LOOP ( 'NONE', ( #14354, #2883, #1196, #4433, #7095 ) ) ;
#11643 = CARTESIAN_POINT ( 'NONE',  ( -2.508389872690818034, 0.2012129740817172052, -2.499130957106830753 ) ) ;
#11644 = EDGE_LOOP ( 'NONE', ( #9953, #10517 ) ) ;
#11645 = CARTESIAN_POINT ( 'NONE',  ( -3.567258970016075725, 5.133675764669605179, 16.99991780678442410 ) ) ;
#11646 = EDGE_CURVE ( 'NONE', #3666, #8289, #6550, .T. ) ;
#11647 = CARTESIAN_POINT ( 'NONE',  ( -1.767766952966369765, 189.1999999978150697, 8.767766952966368876 ) ) ;
#11648 = CARTESIAN_POINT ( 'NONE',  ( -0.2619456584322020221, 5.995505046955617701, 4.026071939286482326 ) ) ;
#11649 = ORIENTED_EDGE ( 'NONE', *, *, #3406, .T. ) ;
#11650 = CARTESIAN_POINT ( 'NONE',  ( 4.435347140100961205, 4.403429997944583008, 11.36765874365829099 ) ) ;
#11651 = CIRCLE ( 'NONE', #3027, 1.999999999999999556 ) ;
#11652 = DIRECTION ( 'NONE',  ( -0.8660254037844266062, -0.5000000000000208722, 0.000000000000000000 ) ) ;
#11653 = CARTESIAN_POINT ( 'NONE',  ( 1.767766952966368654, 1.767766952966369098, -1.800000000000000044 ) ) ;
#11654 = CARTESIAN_POINT ( 'NONE',  ( 3.633127580202256457, 4.776802569231072049, 3.999920388255240322 ) ) ;
#11655 = CARTESIAN_POINT ( 'NONE',  ( 0.000000000000000000, 0.000000000000000000, 0.000000000000000000 ) ) ;
#11656 = CARTESIAN_POINT ( 'NONE',  ( -0.0007128680628333008105, 227.6089742637946642, 5.110086227958842819 ) ) ;
#11657 = CARTESIAN_POINT ( 'NONE',  ( 1.767766952966369098, 188.8999999999999773, 5.232233047033630235 ) ) ;
#11658 = CARTESIAN_POINT ( 'NONE',  ( -1.580502612156455822, 228.6570661798589299, 8.137035460797768849 ) ) ;
#11659 = B_SPLINE_CURVE_WITH_KNOTS ( 'NONE', 3,
 ( #6143, #15683, #13210, #1033, #8451, #13286, #7252, #1189, #8533, #7092, #2222, #10906, #3, #4946, #2467, #4866, #9724, #7330 ),
 .UNSPECIFIED., .F., .F.,
 ( 4, 2, 2, 2, 2, 2, 2, 2, 4 ),
 ( 0.000000000000000000, 0.0003914898357794964652, 0.0007829796715589929304, 0.001174469507338489396, 0.001565959343117985861, 0.001957449178897482326, 0.002348939014676978791, 0.002740428850456475256, 0.003131918686235971722 ),
 .UNSPECIFIED. ) ;
#11660 = UNCERTAINTY_MEASURE_WITH_UNIT (LENGTH_MEASURE( 1.000000000000000082E-05 ), #1945, 'distance_accuracy_value', 'NONE');
#11661 = DIRECTION ( 'NONE',  ( 0.000000000000000000, 0.000000000000000000, 1.000000000000000000 ) ) ;
#11662 = CARTESIAN_POINT ( 'NONE',  ( 0.9740012993921920437, 6.173846968979613159, 24.76164920628449906 ) ) ;
#11663 = CARTESIAN_POINT ( 'NONE',  ( -0.8561741729129455081, 2.066987299999999639, -1.299999998907525267 ) ) ;
#11664 = MECHANICAL_DESIGN_GEOMETRIC_PRESENTATION_REPRESENTATION (  '', ( #2776 ), #4818 ) ;
#11665 = CARTESIAN_POINT ( 'NONE',  ( -2.500000000000000888, 187.5999999999999943, 7.000000000000000000 ) ) ;
#11666 = DIRECTION ( 'NONE',  ( 1.062480551894329776E-17, 2.775557561562888393E-16, -1.000000000000000000 ) ) ;
#11668 = VERTEX_POINT ( 'NONE', #9019 ) ;
#11667 = CARTESIAN_POINT ( 'NONE',  ( -0.8730424326978892813, -5.936362132114493484, 23.99500690218563292 ) ) ;
#11669 = ADVANCED_FACE ( 'NONE', ( #13923 ), #14003, .F. ) ;
#11670 = DIRECTION ( 'NONE',  ( -0.000000000000000000, 1.000000000000000000, -0.000000000000000000 ) ) ;
#11671 =( REPRESENTATION_RELATIONSHIP ('NONE','NONE', #11191, #4596 ) REPRESENTATION_RELATIONSHIP_WITH_TRANSFORMATION ( #14742 )SHAPE_REPRESENTATION_RELATIONSHIP( ) );
#11672 = DIRECTION ( 'NONE',  ( 0.9510565162951499785, 0.3090169943749582204, 0.000000000000000000 ) ) ;
#11673 = CYLINDRICAL_SURFACE ( 'NONE', #13525, 1.999999999999999556 ) ;
#11674 = MECHANICAL_DESIGN_GEOMETRIC_PRESENTATION_REPRESENTATION (  '', ( #12941 ), #8653 ) ;
#11675 = EDGE_CURVE ( 'NONE', #6066, #5999, #408, .T. ) ;
#11676 = DIRECTION ( 'NONE',  ( -1.000000000000000000, 0.000000000000000000, 0.000000000000000000 ) ) ;
#11677 = STYLED_ITEM ( 'NONE', ( #9788 ), #5230 ) ;
#11678 = CARTESIAN_POINT ( 'NONE',  ( -1.035533905932737753, 184.9800000002184959, 4.500000000000000888 ) ) ;
#11679 = CARTESIAN_POINT ( 'NONE',  ( -0.8736516769106569269, 5.936271176698238783, 30.49606771578675080 ) ) ;
#11680 = CARTESIAN_POINT ( 'NONE',  ( 1.814481968427068992, 227.9916212483514641, 6.215192544112370321 ) ) ;
#11681 = FACE_BOUND ( 'NONE', #3528, .T. ) ;
#11682 = CARTESIAN_POINT ( 'NONE',  ( 11.25000000000000355, -1.020968533498575335E-13, 2.000000000000001776 ) ) ;
#11683 = DIRECTION ( 'NONE',  ( -1.000000000000000000, 3.326610055774637112E-18, 1.062480551894331163E-17 ) ) ;
#11684 = EDGE_LOOP ( 'NONE', ( #6558, #6225 ) ) ;
#11685 = CARTESIAN_POINT ( 'NONE',  ( -4.302927372051845722E-16, 184.8499999989074922, 9.066987300000000971 ) ) ;
#11686 = CARTESIAN_POINT ( 'NONE',  ( 1.354942165200771727E-13, 6.000000000000000888, 16.99999999999998579 ) ) ;
#11687 = AXIS2_PLACEMENT_3D ( 'NONE', #15724, #4823, #3539 ) ;
#11688 = EDGE_LOOP ( 'NONE', ( #2018, #9400, #15352, #7793 ) ) ;
#11689 = CARTESIAN_POINT ( 'NONE',  ( -4.286401442266531525, -4.198423832313195270, 5.000000000000004441 ) ) ;
#11690 = CARTESIAN_POINT ( 'NONE',  ( -1.461580736456473240, 184.9499999989075150, 8.461580736456472351 ) ) ;
#11691 = CARTESIAN_POINT ( 'NONE',  ( 5.409274167810672829, 2.597759609440601913, 17.38480617551147844 ) ) ;
#11692 = CARTESIAN_POINT ( 'NONE',  ( -4.743384504624081899E-17, 186.8499999989074922, 4.933012699999999029 ) ) ;
#11693 = CARTESIAN_POINT ( 'NONE',  ( 2.031800924094035195E-13, 6.250000000000000888, 23.49999999999999289 ) ) ;
#11694 = CARTESIAN_POINT ( 'NONE',  ( -2.500000000000000000, 0.000000000000000000, 1.000000002184949777 ) ) ;
#11695 = CARTESIAN_POINT ( 'NONE',  ( 2.082642335314403343E-14, -6.250000000000000888, 31.00000000000000000 ) ) ;
#11696 = CARTESIAN_POINT ( 'NONE',  ( 5.999999999999999112, 185.8606548077538321, 9.048340948986950849 ) ) ;
#11697 = CARTESIAN_POINT ( 'NONE',  ( 2.500000000000000444, 188.7499999978150527, 5.964466094067262247 ) ) ;
#11698 = CARTESIAN_POINT ( 'NONE',  ( -0.8561741729129455081, 2.066987299999999639, -2.699999998907525178 ) ) ;
#11699 = CARTESIAN_POINT ( 'NONE',  ( 5.131373506000491247, 7.062729720844170167, 17.99999999999998934 ) ) ;
#11700 = ORIENTED_EDGE ( 'NONE', *, *, #13730, .T. ) ;
#11701 = ORIENTED_EDGE ( 'NONE', *, *, #10113, .T. ) ;
#11702 = ORIENTED_EDGE ( 'NONE', *, *, #5743, .T. ) ;
#11703 = CARTESIAN_POINT ( 'NONE',  ( 2.692335458626790690, -5.362264153667266164, 24.76239891805597537 ) ) ;
#11704 = CARTESIAN_POINT ( 'NONE',  ( -6.250000000000000888, 0.000000000000000000, 53.67766952966368876 ) ) ;
#11705 = ORIENTED_EDGE ( 'NONE', *, *, #9722, .F. ) ;
#11706 = SURFACE_STYLE_FILL_AREA ( #6715 ) ;
#11707 = CARTESIAN_POINT ( 'NONE',  ( 2.500000000000000444, 1.035533905932737975, -0.9499999978150506230 ) ) ;
#11708 = CARTESIAN_POINT ( 'NONE',  ( 0.7993282387951129442, -5.947240459526509149, 5.614843582169577019 ) ) ;
#11709 = CARTESIAN_POINT ( 'NONE',  ( -4.070051655338043695, -4.744673454622527764, 4.126326713640078303 ) ) ;
#11710 = CARTESIAN_POINT ( 'NONE',  ( 1.461580736456472573, 185.1499999989075320, 8.461580736456474128 ) ) ;
#11711 = CARTESIAN_POINT ( 'NONE',  ( 1.035533905932739085, -2.500000000000000000, -1.243000000021849960 ) ) ;
#11712 = FACE_OUTER_BOUND ( 'NONE', #7731, .T. ) ;
#11713 = SHAPE_DEFINITION_REPRESENTATION ( #13501, #3660 ) ;
#11714 = CARTESIAN_POINT ( 'NONE',  ( 2.066987300000000083, -0.8561741729129449530, 0.8000000010924747107 ) ) ;
#11715 = CARTESIAN_POINT ( 'NONE',  ( -2.500000000000000888, 189.1699999975965341, 7.000000000000000000 ) ) ;
#11716 = CARTESIAN_POINT ( 'NONE',  ( 2.923059718105053051, 227.5089953743221258, 7.973592892444406388 ) ) ;
#11717 = FACE_OUTER_BOUND ( 'NONE', #806, .T. ) ;
#11718 = EDGE_LOOP ( 'NONE', ( #13384, #13775, #9479, #5869 ) ) ;
#11719 = CARTESIAN_POINT ( 'NONE',  ( -1.370134448080163825, 2.110273492104576043, -2.498966192944565456 ) ) ;
#11720 = ORIENTED_EDGE ( 'NONE', *, *, #1525, .T. ) ;
#11721 = EDGE_CURVE ( 'NONE', #9483, #12468, #823, .T. ) ;
#11722 = CARTESIAN_POINT ( 'NONE',  ( -0.9999505860952755398, 6.169489349035817582, 11.63105903165808108 ) ) ;
#11723 = CYLINDRICAL_SURFACE ( 'NONE', #6361, 1.000000000000000222 ) ;
#11724 = CARTESIAN_POINT ( 'NONE',  ( -0.1323933160975646617, 6.000000000000000000, 6.000000000000003553 ) ) ;
#11725 = ORIENTED_EDGE ( 'NONE', *, *, #1525, .F. ) ;
#11726 = CARTESIAN_POINT ( 'NONE',  ( -5.935543223013841185, 0.8771126767608004027, 17.99999999999998934 ) ) ;
#11727 = LINE ( 'NONE', #831, #11979 ) ;
#11728 = CARTESIAN_POINT ( 'NONE',  ( 3.883716939929057421, -4.898343590941192538, 17.02640428276698259 ) ) ;
#11729 = CARTESIAN_POINT ( 'NONE',  ( 1.767766952966369320, -1.767766952966368654, -2.000000000000000444 ) ) ;
#11730 = CARTESIAN_POINT ( 'NONE',  ( -3.159082487394891281, -5.393634094348267460, 25.29954462468842635 ) ) ;
#11731 = SURFACE_STYLE_FILL_AREA ( #8084 ) ;
#11732 = DIRECTION ( 'NONE',  ( 0.000000000000000000, 0.000000000000000000, -1.000000000000000000 ) ) ;
#11733 = PRODUCT_DEFINITION_SHAPE ( 'NONE', 'NONE',  #15762 ) ;
#11734 = CARTESIAN_POINT ( 'NONE',  ( -2.500000000000000888, 188.4500000000000171, 8.035533905932737753 ) ) ;
#11735 = ADVANCED_FACE ( 'NONE', ( #1909 ), #5587, .F. ) ;
#11736 = CARTESIAN_POINT ( 'NONE',  ( -0.9967757174687167376, 228.8247258804818216, 8.621246238880397428 ) ) ;
#11737 = CARTESIAN_POINT ( 'NONE',  ( 7.180990026460747799, -3.384707322287378695, 31.00000000000000000 ) ) ;
#11738 = CARTESIAN_POINT ( 'NONE',  ( -5.782947755040646953, 1.603807858344055370, 18.97398020122238194 ) ) ;
#11739 = EDGE_CURVE ( 'NONE', #512, #10893, #11296, .T. ) ;
#11740 = CARTESIAN_POINT ( 'NONE',  ( 0.05969309337805784460, 188.9999999999999432, 4.500684243071288115 ) ) ;
#11741 = VECTOR ( 'NONE', #3863, 1000.000000000000114 ) ;
#11742 = CARTESIAN_POINT ( 'NONE',  ( 1.035533905932738197, 186.2500000000000000, 9.500000000000003553 ) ) ;
#11743 = CARTESIAN_POINT ( 'NONE',  ( -3.567624405365465101, 5.133384272590623354, 25.49995078984292007 ) ) ;
#11745 = VERTEX_POINT ( 'NONE', #12805 ) ;
#11744 = CARTESIAN_POINT ( 'NONE',  ( 2.031800923283433283E-13, -6.000000000000000888, 23.49999999999999289 ) ) ;
#11746 = CARTESIAN_POINT ( 'NONE',  ( -5.769755079862278535, 2.405651898699073588, 18.87305891554299464 ) ) ;
#11747 = VERTEX_POINT ( 'NONE', #6782 ) ;
#11748 = DIRECTION ( 'NONE',  ( 0.5877852522924802425, -0.8090169943749422332, 0.000000000000000000 ) ) ;
#11749 = CARTESIAN_POINT ( 'NONE',  ( -2.660650785759065329, 227.7358070380394963, 8.640981985597708359 ) ) ;
#11750 = CARTESIAN_POINT ( 'NONE',  ( 0.8841844500102366000, 190.0747139113696846, 4.330645362478406923 ) ) ;
#11751 = CARTESIAN_POINT ( 'NONE',  ( 1.767766952966368654, 185.4300000002185129, 8.767766952966368876 ) ) ;
#11752 = CARTESIAN_POINT ( 'NONE',  ( -5.531623157106165145, -2.327208526676436851, 5.873647046844243214 ) ) ;
#11753 = CARTESIAN_POINT ( 'NONE',  ( 1.692341931978252223, 227.9167330860961442, 5.998911260178718230 ) ) ;
#11754 = CARTESIAN_POINT ( 'NONE',  ( 6.020822430078789367, 1.681351817312415564, 10.52591457665827335 ) ) ;
#11755 = FACE_OUTER_BOUND ( 'NONE', #9897, .T. ) ;
#11756 = FACE_OUTER_BOUND ( 'NONE', #5362, .T. ) ;
#11757 = ORIENTED_EDGE ( 'NONE', *, *, #4351, .T. ) ;
#11758 = CARTESIAN_POINT ( 'NONE',  ( 1.461580736456473462, 184.3499999989074922, 5.538419263543526760 ) ) ;
#11759 = CARTESIAN_POINT ( 'NONE',  ( 3.735808404764985546, 4.696639218303137575, 30.02601979877761451 ) ) ;
#11760 = EDGE_LOOP ( 'NONE', ( #7566, #4987, #11141, #11626 ) ) ;
#11761 = ADVANCED_FACE ( 'NONE', ( #7807 ), #717, .F. ) ;
#11762 = CARTESIAN_POINT ( 'NONE',  ( 1.035533905932738197, 186.2500000000000000, 9.500000000000000000 ) ) ;
#11763 = CARTESIAN_POINT ( 'NONE',  ( -1.461580736456472795, 184.7499999989074979, 5.538419263543527649 ) ) ;
#11764 = CARTESIAN_POINT ( 'NONE',  ( 2.930600586412840602, 5.520563544161817937, 17.49691356133953946 ) ) ;
#11765 = CARTESIAN_POINT ( 'NONE',  ( 0.8561741729129456191, 187.5999999989074922, 4.933012699999999029 ) ) ;
#11766 = CARTESIAN_POINT ( 'NONE',  ( -3.567258970015892761, -5.133675764669733965, 6.000082193215567905 ) ) ;
#11767 = CARTESIAN_POINT ( 'NONE',  ( -1.767766952966368432, -1.767766952966369320, -0.4999999978150501123 ) ) ;
#11768 = CARTESIAN_POINT ( 'NONE',  ( 2.692143549875417374, -5.362363179736472141, 11.23805675996853104 ) ) ;
#11769 = CARTESIAN_POINT ( 'NONE',  ( 5.999999999999999112, 187.2933328889893403, 9.583808270834989429 ) ) ;
#11770 = CARTESIAN_POINT ( 'NONE',  ( 2.082642335314403343E-14, -6.250000000000000888, 32.00000000000000000 ) ) ;
#11771 = CARTESIAN_POINT ( 'NONE',  ( -2.066987299999999639, 0.8561741729129452860, -2.599999998907525089 ) ) ;
#11772 = AXIS2_PLACEMENT_3D ( 'NONE', #3095, #2125, #4524 ) ;
#11773 = LINE ( 'NONE', #14308, #1599 ) ;
#11774 = EDGE_LOOP ( 'NONE', ( #11447, #641, #7897, #821 ) ) ;
#11775 = ORIENTED_EDGE ( 'NONE', *, *, #11675, .F. ) ;
#11776 = ORIENTED_EDGE ( 'NONE', *, *, #14856, .F. ) ;
#11777 = CARTESIAN_POINT ( 'NONE',  ( 1.461580736456473018, 184.5499999989075093, 5.538419263543527649 ) ) ;
#11778 = CARTESIAN_POINT ( 'NONE',  ( 1.221831151830281126, 228.7817678443040563, 8.497180980233151715 ) ) ;
#11779 = VERTEX_POINT ( 'NONE', #12578 ) ;
#11780 = EDGE_CURVE ( 'NONE', #13950, #878, #8522, .T. ) ;
#11781 = CARTESIAN_POINT ( 'NONE',  ( -1.530808498934191571E-16, 2.500000000000000000, 0.8000000021849495990 ) ) ;
#11782 = CARTESIAN_POINT ( 'NONE',  ( 0.6152055445546467105, -5.969096820685153126, 5.799049686702669071 ) ) ;
#11783 = CARTESIAN_POINT ( 'NONE',  ( 3.779681992289640302, 4.979315417304017721, 25.49995078984292718 ) ) ;
#11784 = CARTESIAN_POINT ( 'NONE',  ( 2.066987300000000083, 184.4499999989075150, 7.000000000000000000 ) ) ;
#11785 = CARTESIAN_POINT ( 'NONE',  ( 4.592425496802573972E-16, -2.500000000000000000, -0.4930000000218495715 ) ) ;
#11786 = AXIS2_PLACEMENT_3D ( 'NONE', #758, #13001, #10626 ) ;
#11787 = CARTESIAN_POINT ( 'NONE',  ( 6.176542424588118863, -0.9554180641285446862, 4.869393092765015751 ) ) ;
#11788 = CONTEXT_DEPENDENT_SHAPE_REPRESENTATION ( #2923, #11852 ) ;
#11789 = CARTESIAN_POINT ( 'NONE',  ( -0.8561741729129458411, -2.066987299999999195, 1.400000001092474911 ) ) ;
#11790 = CARTESIAN_POINT ( 'NONE',  ( -5.531209434046327367, -2.328189801702647443, 4.126962209729496678 ) ) ;
#11791 = CARTESIAN_POINT ( 'NONE',  ( 0.6843230633849453071, 226.3504559366005537, 4.561183366923295068 ) ) ;
#11792 = CARTESIAN_POINT ( 'NONE',  ( 4.290381260516173967, 4.545736887716300245, 18.61517780375843145 ) ) ;
#11793 = VERTEX_POINT ( 'NONE', #9316 ) ;
#11794 = VERTEX_POINT ( 'NONE', #4543 ) ;
#11795 = CARTESIAN_POINT ( 'NONE',  ( 0.6156133477426980471, 6.220296490279942248, 31.79872387345512053 ) ) ;
#11796 = EDGE_CURVE ( 'NONE', #12482, #8538, #11842, .T. ) ;
#11797 = CARTESIAN_POINT ( 'NONE',  ( 6.176542424588149949, -0.9554180641283412934, 24.49999999999999289 ) ) ;
#11798 = CARTESIAN_POINT ( 'NONE',  ( 6.768587589771821120E-14, -6.250000000000000888, 12.49999999999998401 ) ) ;
#11799 = EDGE_LOOP ( 'NONE', ( #15650, #12991, #6128, #2407, #4471, #5224, #1859 ) ) ;
#11800 = CARTESIAN_POINT ( 'NONE',  ( 2.996920846510460201, 5.485395142346805031, 10.88558052754513383 ) ) ;
#11801 = CARTESIAN_POINT ( 'NONE',  ( -0.7988860301922200424, -6.199427171881335852, 4.384555805361945779 ) ) ;
#11802 = FACE_BOUND ( 'NONE', #11319, .T. ) ;
#11803 = CARTESIAN_POINT ( 'NONE',  ( -2.500000000000000000, -1.035533905932739307, -1.349999997815050090 ) ) ;
#11804 = CARTESIAN_POINT ( 'NONE',  ( -1.767766952966368432, -1.767766952966369320, 1.000000000000000000 ) ) ;
#11805 = CARTESIAN_POINT ( 'NONE',  ( -2.931212650151761245, -5.520239928492765458, 25.00425949503010514 ) ) ;
#11806 = CARTESIAN_POINT ( 'NONE',  ( 5.487097279078403389, 2.429065649168880014, 5.799520541027148646 ) ) ;
#11807 = CARTESIAN_POINT ( 'NONE',  ( 2.500000000000000444, 188.8499999999999659, 5.964466094067262247 ) ) ;
#11808 = EDGE_CURVE ( 'NONE', #3801, #10844, #6328, .T. ) ;
#11809 = CARTESIAN_POINT ( 'NONE',  ( -1.973877840180719989, 228.3455757694837303, 7.237433389386023208 ) ) ;
#11810 = CARTESIAN_POINT ( 'NONE',  ( 5.665824935993602374, 1.978765057080938528, 10.50004946353775281 ) ) ;
#11811 = CARTESIAN_POINT ( 'NONE',  ( -1.929793783875213720, 189.4086015753950960, 4.698290738201920114 ) ) ;
#11812 = CARTESIAN_POINT ( 'NONE',  ( 1.767766952966369098, 186.5000000000000000, 5.232233047033630235 ) ) ;
#11813 = CARTESIAN_POINT ( 'NONE',  ( 3.158296126777728752, -5.394094919772149055, 25.29887838423338309 ) ) ;
#11815 = ORIENTED_EDGE ( 'NONE', *, *, #11085, .F. ) ;
#11814 = CARTESIAN_POINT ( 'NONE',  ( -13.50000000000000000, 2.000000000000000000, 2.479909768273400161E-15 ) ) ;
#11816 = CARTESIAN_POINT ( 'NONE',  ( 0.8499999999999896527, 0.4000000000000062395, 2.619018321873338273 ) ) ;
#11817 = DIRECTION ( 'NONE',  ( 0.8090169943749421222, 0.5877852522924802425, 0.000000000000000000 ) ) ;
#11818 = CARTESIAN_POINT ( 'NONE',  ( -2.990970242699510173, 227.3667325949381564, 7.554906020068777650 ) ) ;
#11819 = EDGE_CURVE ( 'NONE', #7314, #1678, #3259, .T. ) ;
#11820 = CARTESIAN_POINT ( 'NONE',  ( 0.2560036892252900986, 189.0000000000580371, 4.506310952893917587 ) ) ;
#11821 = CARTESIAN_POINT ( 'NONE',  ( -2.500000000000000444, 185.9300000002185129, 7.000000000000000000 ) ) ;
#11822 = CARTESIAN_POINT ( 'NONE',  ( -4.152999119457993160, 4.671604476854340326, 5.800265150176763918 ) ) ;
#11823 = EDGE_CURVE ( 'NONE', #15063, #3801, #12903, .T. ) ;
#11824 = CARTESIAN_POINT ( 'NONE',  ( 1.989829716803914739, 228.2822890550965553, 7.054657748597916722 ) ) ;
#11825 = FACE_BOUND ( 'NONE', #1309, .T. ) ;
#11826 = CARTESIAN_POINT ( 'NONE',  ( -5.648559266344554075, 2.676764518775872848, 4.386038205919296828 ) ) ;
#11827 = CARTESIAN_POINT ( 'NONE',  ( -2.849269941561927588, -5.281123252784065691, 30.38480617551148910 ) ) ;
#11828 = ORIENTED_EDGE ( 'NONE', *, *, #5465, .T. ) ;
#11829 = CARTESIAN_POINT ( 'NONE',  ( 2.066987300000000971, 185.8999999989075036, 6.143825827087054492 ) ) ;
#11830 = CARTESIAN_POINT ( 'NONE',  ( -2.500000000000000444, 184.4000000000000057, 7.000000000000000000 ) ) ;
#11831 = VERTEX_POINT ( 'NONE', #3338 ) ;
#11832 = CARTESIAN_POINT ( 'NONE',  ( 0.000000000000000000, 0.000000000000000000, 0.000000000000000000 ) ) ;
#11834 = CARTESIAN_POINT ( 'NONE',  ( -4.286401442266607908, 4.198423832313116222, 31.13064961348856130 ) ) ;
#11833 = B_SPLINE_CURVE_WITH_KNOTS ( 'NONE', 3,
 ( #13068, #8311, #15627, #9502, #13149, #7200, #2251, #2328, #9422, #15473, #4893, #1138, #9581, #11795, #12041, #4650, #14508, #982 ),
 .UNSPECIFIED., .F., .F.,
 ( 4, 2, 2, 2, 2, 2, 2, 2, 4 ),
 ( 0.003131490185286055824, 0.003522829482338662825, 0.003914168779391269393, 0.004305508076443876828, 0.004696847373496483395, 0.005088186670549079554, 0.005479525967601676581, 0.005870865264654273608, 0.006262204561706869767 ),
 .UNSPECIFIED. ) ;
#11835 = VECTOR ( 'NONE', #7692, 1000.000000000000000 ) ;
#11836 = CARTESIAN_POINT ( 'NONE',  ( 0.5030929395821142069, 6.230885867001139999, 10.62600319116548597 ) ) ;
#11837 = CARTESIAN_POINT ( 'NONE',  ( 2.066987299999999639, 188.1999999989075150, 7.856174172912946396 ) ) ;
#11838 = CARTESIAN_POINT ( 'NONE',  ( 3.736691294293485566, -4.695920479336326281, 30.02641404563305372 ) ) ;
#11839 = CARTESIAN_POINT ( 'NONE',  ( -1.767766952966369098, 1.767766952966369098, 0.1000000021849497545 ) ) ;
#11840 = DIRECTION ( 'NONE',  ( 6.123233995736603333E-17, -1.000000000000000000, 3.749399456655569780E-33 ) ) ;
#11841 = CARTESIAN_POINT ( 'NONE',  ( 5.999999999999999112, 194.5935680195190116, 12.11154058223188379 ) ) ;
#11842 = LINE ( 'NONE', #13119, #10794 ) ;
#11843 = CARTESIAN_POINT ( 'NONE',  ( 2.066987300000000083, -0.8561741729129449530, -2.199999998907525178 ) ) ;
#11844 = PLANE ( 'NONE',  #7703 ) ;
#11845 = ORIENTED_EDGE ( 'NONE', *, *, #13677, .T. ) ;
#11846 = EDGE_LOOP ( 'NONE', ( #14311, #15547, #9704, #4398 ) ) ;
#11847 = EDGE_LOOP ( 'NONE', ( #13839, #5669, #4486, #15198 ) ) ;
#11848 = CARTESIAN_POINT ( 'NONE',  ( 4.267558728637114385, -4.217879122113883383, 24.76382603205594179 ) ) ;
#11849 = CARTESIAN_POINT ( 'NONE',  ( 0.000000000000000000, 182.0000000000000000, -3.000000000000000888 ) ) ;
#11850 = ORIENTED_EDGE ( 'NONE', *, *, #12219, .F. ) ;
#11851 = EDGE_CURVE ( 'NONE', #14331, #7444, #10081, .T. ) ;
#11852 = PRODUCT_DEFINITION_SHAPE ( 'NONE', 'NONE',  #15734 ) ;
#11853 = CARTESIAN_POINT ( 'NONE',  ( -2.500000000000000000, -1.035533905932739307, -2.149999997815051245 ) ) ;
#11854 = CARTESIAN_POINT ( 'NONE',  ( -0.6139908388538884987, 5.969238533166634220, 23.69977627912011897 ) ) ;
#11855 = DIRECTION ( 'NONE',  ( 1.000000000000000000, 0.000000000000000000, 0.000000000000000000 ) ) ;
#11856 = CARTESIAN_POINT ( 'NONE',  ( 2.500000000000000444, 187.9499999978150697, 5.964466094067262247 ) ) ;
#11857 = CARTESIAN_POINT ( 'NONE',  ( -1.767766952966369098, 1.767766952966369098, -0.7930000000218494494 ) ) ;
#11858 = CARTESIAN_POINT ( 'NONE',  ( 5.985119669071112369, -1.805077827356573517, 4.000082581897114409 ) ) ;
#11859 = SHAPE_DEFINITION_REPRESENTATION ( #10829, #9569 ) ;
#11860 = CARTESIAN_POINT ( 'NONE',  ( -0.8561741729129455081, 2.066987299999999639, -0.4999999989075253337 ) ) ;
#11861 = EDGE_CURVE ( 'NONE', #5534, #14733, #3664, .T. ) ;
#11862 = B_SPLINE_CURVE_WITH_KNOTS ( 'NONE', 3,
 ( #1617, #425, #9183, #10372, #11328, #15150, #4243, #9112, #14997, #13941, #3052, #12745, #1849, #3279, #3204, #12822, #14247, #5835 ),
 .UNSPECIFIED., .F., .F.,
 ( 4, 2, 2, 2, 2, 2, 2, 2, 4 ),
 ( 0.003131918686235958711, 0.003523310662250251149, 0.003914702638264542719, 0.004306094614278835157, 0.004697486590293127595, 0.005088878566307419166, 0.005480270542321710736, 0.005871662518336002307, 0.006263054494350293877 ),
 .UNSPECIFIED. ) ;
#11863 = CARTESIAN_POINT ( 'NONE',  ( 6.123233995736766282E-16, 22.00000000000000000, 5.000000000000000000 ) ) ;
#11864 = CARTESIAN_POINT ( 'NONE',  ( 2.993808330938719564, 227.3535049858431591, 7.515946948957763496 ) ) ;
#11865 = CARTESIAN_POINT ( 'NONE',  ( 2.840966774240103465, 5.567223638426939125, 18.26190213084012015 ) ) ;
#11866 = ORIENTED_EDGE ( 'NONE', *, *, #201, .F. ) ;
#11867 = CARTESIAN_POINT ( 'NONE',  ( -5.665308849928780255, 1.980336949702632632, 25.49992002356261622 ) ) ;
#11868 = CARTESIAN_POINT ( 'NONE',  ( 4.416397290909769069, 4.422724436066569176, 24.23620383159193636 ) ) ;
#11869 = EDGE_LOOP ( 'NONE', ( #3060, #11911 ) ) ;
#11870 = EDGE_LOOP ( 'NONE', ( #7002, #9084, #14964, #5415 ) ) ;
#11871 = CARTESIAN_POINT ( 'NONE',  ( -5.648794263291742723, -2.676232015153619415, 30.38558052754516225 ) ) ;
#11872 =( REPRESENTATION_RELATIONSHIP ('NONE','NONE', #11191, #4596 ) REPRESENTATION_RELATIONSHIP_WITH_TRANSFORMATION ( #11229 )SHAPE_REPRESENTATION_RELATIONSHIP( ) );
#11873 =( LENGTH_UNIT ( ) NAMED_UNIT ( * ) SI_UNIT ( .MILLI., .METRE. ) );
#11874 = CARTESIAN_POINT ( 'NONE',  ( 1.035533905932738419, 185.4500000000000171, 9.500000000000000000 ) ) ;
#11875 = VERTEX_POINT ( 'NONE', #15522 ) ;
#11876 = CARTESIAN_POINT ( 'NONE',  ( -5.984759433607027113, 1.806271833852240105, 32.00008219321556169 ) ) ;
#11877 = UNCERTAINTY_MEASURE_WITH_UNIT (LENGTH_MEASURE( 1.000000000000000082E-05 ), #13761, 'distance_accuracy_value', 'NONE');
#11878 = CARTESIAN_POINT ( 'NONE',  ( -0.2623718222035099079, -6.245654667075784872, 4.026278297138354390 ) ) ;
#11879 = CARTESIAN_POINT ( 'NONE',  ( -0.6144300524831621813, -6.220417338033072951, 23.70033372175933550 ) ) ;
#11880 = DIRECTION ( 'NONE',  ( -0.000000000000000000, -1.000000000000000000, -0.000000000000000000 ) ) ;
#11881 = CARTESIAN_POINT ( 'NONE',  ( -1.767766952966368432, -1.767766952966369320, -2.200000000000000178 ) ) ;
#11882 = CARTESIAN_POINT ( 'NONE',  ( 0.000000000000000000, 0.000000000000000000, 0.000000000000000000 ) ) ;
#11883 = AXIS2_PLACEMENT_3D ( 'NONE', #7317, #10967, #1255 ) ;
#11884 = CARTESIAN_POINT ( 'NONE',  ( 0.09025563639527389714, 0.4000000000000047962, -2.551758345435058306 ) ) ;
#11885 = CARTESIAN_POINT ( 'NONE',  ( 9.825582188149883933E-17, 184.8999999978150584, 4.500000000000000000 ) ) ;
#11886 = VECTOR ( 'NONE', #5838, 1000.000000000000000 ) ;
#11887 = CARTESIAN_POINT ( 'NONE',  ( 1.326034168411047265, 228.1562120337857777, 9.877435289762864556 ) ) ;
#11888 = CARTESIAN_POINT ( 'NONE',  ( 5.531796221294864147, 2.326749136277247221, 10.62621569129737331 ) ) ;
#11889 = CARTESIAN_POINT ( 'NONE',  ( -1.482782158083479018, 190.0495907483965823, 4.595143857422339551 ) ) ;
#11890 = ORIENTED_EDGE ( 'NONE', *, *, #4392, .F. ) ;
#11891 = DIRECTION ( 'NONE',  ( 0.000000000000000000, 0.000000000000000000, -1.000000000000000000 ) ) ;
#11892 = CARTESIAN_POINT ( 'NONE',  ( 1.500000000000000000, -9.750000000000003553, 0.000000000000000000 ) ) ;
#11893 = AXIS2_PLACEMENT_3D ( 'NONE', #2812, #7582, #8712 ) ;
#11895 = ORIENTED_EDGE ( 'NONE', *, *, #1627, .T. ) ;
#11894 = CARTESIAN_POINT ( 'NONE',  ( -0.5042987395405625906, -5.979983180450094693, 25.37329304179976930 ) ) ;
#11896 = CARTESIAN_POINT ( 'NONE',  ( 0.005811324839270699469, -0.3999999999999993006, 2.486892833834318139 ) ) ;
#11897 = PRESENTATION_LAYER_ASSIGNMENT (  '', '', ( #8367 ) ) ;
#11898 = B_SPLINE_CURVE_WITH_KNOTS ( 'NONE', 3,
 ( #10310, #11417, #4104, #10003, #518, #10077, #4180, #11264, #2912, #7684, #12532, #8974, #14850, #365, #13877, #9051, #7762, #7843 ),
 .UNSPECIFIED., .F., .F.,
 ( 4, 2, 2, 2, 2, 2, 2, 2, 4 ),
 ( 0.000000000000000000, 0.0003914898357794980915, 0.0007829796715589961830, 0.001174469507338494166, 0.001565959343117991282, 0.001957449178897488831, 0.002348939014676985730, 0.002740428850456482629, 0.003131918686235979962 ),
 .UNSPECIFIED. ) ;
#11899 = CARTESIAN_POINT ( 'NONE',  ( -5.131373506000878493, 7.062729720843910819, 24.49999999999999289 ) ) ;
#11900 = CARTESIAN_POINT ( 'NONE',  ( -1.461580736456472795, 1.461580736456472795, -2.849999998907525089 ) ) ;
#11901 = CARTESIAN_POINT ( 'NONE',  ( 0.8561741729129463963, -2.066987299999999195, 1.700000001092474733 ) ) ;
#11902 = CARTESIAN_POINT ( 'NONE',  ( -2.148870826313457716, 226.6164604241740506, 5.345220325073331225 ) ) ;
#11903 = CARTESIAN_POINT ( 'NONE',  ( 5.616116467183688954, 2.743044348085479367, 25.00425949503011225 ) ) ;
#11904 = CARTESIAN_POINT ( 'NONE',  ( -1.767766952966369098, 184.2300000002184959, 5.232233047033630235 ) ) ;
#11905 = CARTESIAN_POINT ( 'NONE',  ( -0.5214357632711458246, 228.8948738370037290, 8.823837538292856664 ) ) ;
#11906 = CARTESIAN_POINT ( 'NONE',  ( -0.9962072163307928996, 227.6960174938032537, 5.361472040843871412 ) ) ;
#11908 = CARTESIAN_POINT ( 'NONE',  ( 5.725930890718300859, 2.506952462184107500, 10.70066851092422411 ) ) ;
#11907 = MECHANICAL_DESIGN_GEOMETRIC_PRESENTATION_REPRESENTATION (  '', ( #7858 ), #14444 ) ;
#11909 = CARTESIAN_POINT ( 'NONE',  ( 2.066987299999999639, 0.8561741729129456191, -0.4999999989075253892 ) ) ;
#11910 = CARTESIAN_POINT ( 'NONE',  ( -2.668367453516648613, -5.373994336898124224, 30.86760611998365178 ) ) ;
#11911 = ORIENTED_EDGE ( 'NONE', *, *, #7936, .T. ) ;
#11912 = CARTESIAN_POINT ( 'NONE',  ( -1.461580736456473240, 187.7499999989075263, 5.538419263543526760 ) ) ;
#11913 = DIRECTION ( 'NONE',  ( 0.000000000000000000, 0.000000000000000000, 1.000000000000000000 ) ) ;
#11914 = EDGE_CURVE ( 'NONE', #1447, #5635, #12565, .T. ) ;
#11915 = ORIENTED_EDGE ( 'NONE', *, *, #12695, .F. ) ;
#11916 = EDGE_CURVE ( 'NONE', #8921, #13014, #12956, .T. ) ;
#11917 = DIRECTION ( 'NONE',  ( 0.000000000000000000, 0.000000000000000000, 1.000000000000000000 ) ) ;
#11918 = CARTESIAN_POINT ( 'NONE',  ( 0.000000000000000000, 6.250000000000000888, 6.000000000000005329 ) ) ;
#11919 = CARTESIAN_POINT ( 'NONE',  ( 0.8561741729129456191, 184.5999999989075206, 4.933012699999999029 ) ) ;
#11920 = EDGE_CURVE ( 'NONE', #7970, #9955, #5760, .T. ) ;
#11921 = CARTESIAN_POINT ( 'NONE',  ( 5.782895619916181396, 1.604017620857993709, 17.02591947216898305 ) ) ;
#11922 = CARTESIAN_POINT ( 'NONE',  ( -5.285485590866834116E-16, 186.4499999989075150, 9.066987300000000971 ) ) ;
#11923 = CARTESIAN_POINT ( 'NONE',  ( 3.421280866381030350, 4.930711975950989867, 19.00004932073311181 ) ) ;
#11924 = CARTESIAN_POINT ( 'NONE',  ( 1.035533905932737531, 2.500000000000000444, -0.8499999978150500901 ) ) ;
#11925 = CARTESIAN_POINT ( 'NONE',  ( -6.176542424588106428, -0.9554180641286325049, 4.867658743658319409 ) ) ;
#11926 = B_SPLINE_CURVE_WITH_KNOTS ( 'NONE', 3,
 ( #4083, #12742, #8877, #7589, #12437, #2894, #8796 ),
 .UNSPECIFIED., .F., .F.,
 ( 4, 3, 4 ),
 ( 0.004378233155234299845, 0.004805482862474828344, 0.005139916140522488193 ),
 .UNSPECIFIED. ) ;
#11927 = CARTESIAN_POINT ( 'NONE',  ( 0.000000000000000000, 215.3885876087883275, 13.29602556813378733 ) ) ;
#11928 = CARTESIAN_POINT ( 'NONE',  ( -1.767766952966369542, 185.1999999978150697, 8.767766952966368876 ) ) ;
#11929 = CARTESIAN_POINT ( 'NONE',  ( 1.353717517954364224E-13, -6.000000000000000888, 18.99999999999998934 ) ) ;
#11930 = ORIENTED_EDGE ( 'NONE', *, *, #10002, .F. ) ;
#11931 = PRESENTATION_LAYER_ASSIGNMENT (  '', '', ( #12941 ) ) ;
#11932 = ORIENTED_EDGE ( 'NONE', *, *, #8439, .F. ) ;
#11933 = EDGE_CURVE ( 'NONE', #2475, #9302, #7935, .T. ) ;
#11934 = ORIENTED_EDGE ( 'NONE', *, *, #7561, .F. ) ;
#11935 = CARTESIAN_POINT ( 'NONE',  ( -1.461580736456472795, 185.5499999989075093, 5.538419263543527649 ) ) ;
#11936 = CARTESIAN_POINT ( 'NONE',  ( 6.768587589771821120E-14, -6.250000000000000888, 11.49999999999998224 ) ) ;
#11937 = VERTEX_POINT ( 'NONE', #14559 ) ;
#11938 = EDGE_CURVE ( 'NONE', #7643, #1252, #12202, .T. ) ;
#11939 = CARTESIAN_POINT ( 'NONE',  ( -1.767766952966368432, -1.767766952966369320, -1.299999997815050712 ) ) ;
#11940 = CARTESIAN_POINT ( 'NONE',  ( 6.176542424588125080, 0.9554180641284967246, 18.13060690723496649 ) ) ;
#11941 = DIRECTION ( 'NONE',  ( -1.000000000000000000, 3.326610055774637112E-18, 1.062480551894331163E-17 ) ) ;
#11942 = CARTESIAN_POINT ( 'NONE',  ( -0.8561741729129456191, 187.8999999989075320, 4.933012699999999029 ) ) ;
#11943 = VECTOR ( 'NONE', #2191, 1000.000000000000114 ) ;
#11944 = CARTESIAN_POINT ( 'NONE',  ( -1.767766952966369098, 1.767766952966369098, 0.8069999999781504174 ) ) ;
#11945 = DIRECTION ( 'NONE',  ( 0.9510565162951499785, 0.3090169943749582204, 0.000000000000000000 ) ) ;
#11946 = CONTEXT_DEPENDENT_SHAPE_REPRESENTATION ( #15143, #3098 ) ;
#11947 = CARTESIAN_POINT ( 'NONE',  ( -2.066987299999999639, 0.8561741729129452860, 2.200000001092475177 ) ) ;
#11948 = CARTESIAN_POINT ( 'NONE',  ( 2.817313151351169331, -5.579000502529441796, 31.00000000000000000 ) ) ;
#11949 = CARTESIAN_POINT ( 'NONE',  ( 2.550395957922052759, 226.7806086135062458, 5.828878098564913124 ) ) ;
#11950 = CARTESIAN_POINT ( 'NONE',  ( 5.726049995854432417, 2.506679546901958489, 5.799544624688433458 ) ) ;
#11951 = ORIENTED_EDGE ( 'NONE', *, *, #1242, .F. ) ;
#11952 = EDGE_LOOP ( 'NONE', ( #7677, #9559 ) ) ;
#11953 = DIRECTION ( 'NONE',  ( -1.000000000000000000, 0.000000000000000000, 0.000000000000000000 ) ) ;
#11954 = ORIENTED_EDGE ( 'NONE', *, *, #2508, .T. ) ;
#11955 = EDGE_LOOP ( 'NONE', ( #11453, #622, #14961, #8419 ) ) ;
#11956 = CARTESIAN_POINT ( 'NONE',  ( -6.081509788407734263, -1.446521464462734885, 30.12618035954928075 ) ) ;
#11957 = CARTESIAN_POINT ( 'NONE',  ( -3.158825713737613228, -5.393784879207096594, 23.70066851092423477 ) ) ;
#11958 = CARTESIAN_POINT ( 'NONE',  ( -4.286401442266675410, -4.198423832313046944, 24.49999999999999289 ) ) ;
#11959 = EDGE_CURVE ( 'NONE', #2808, #1290, #6377, .T. ) ;
#11960 = EDGE_LOOP ( 'NONE', ( #7711, #5284 ) ) ;
#11961 = CARTESIAN_POINT ( 'NONE',  ( -6.081464507797624819, -1.446657058464231538, 31.87380055247395561 ) ) ;
#11962 = CARTESIAN_POINT ( 'NONE',  ( 5.747343991580227573, -1.727858744772131194, 17.00007997643736957 ) ) ;
#11963 = CARTESIAN_POINT ( 'NONE',  ( -4.322356511625935482, 7.650514973136391284, 24.49999999999999289 ) ) ;
#11964 = CARTESIAN_POINT ( 'NONE',  ( -3.459447313391904366, -5.206669755180949544, 18.97400098023329562 ) ) ;
#11965 = EDGE_CURVE ( 'NONE', #4625, #10924, #7840, .T. ) ;
#11966 = CARTESIAN_POINT ( 'NONE',  ( 5.486982057989157724, 2.429327048029951364, 30.20068193741824913 ) ) ;
#11967 = CARTESIAN_POINT ( 'NONE',  ( -1.084202172485504434E-16, 3.464101615137754830, -2.500000000000000000 ) ) ;
#11968 = DIRECTION ( 'NONE',  ( 1.000000000000000000, 0.000000000000000000, 0.000000000000000000 ) ) ;
#11969 = CARTESIAN_POINT ( 'NONE',  ( 2.500000000000000000, 188.6499999978150584, 8.035533905932739529 ) ) ;
#11970 = CARTESIAN_POINT ( 'NONE',  ( 2.994032664863047533, 227.2266946368854690, 7.142638454998203379 ) ) ;
#11971 = CARTESIAN_POINT ( 'NONE',  ( 2.782468714962362366, 5.316055268221441032, 31.50389795015983552 ) ) ;
#11972 = CARTESIAN_POINT ( 'NONE',  ( -0.6578658431935565654, 189.0000000007884466, 4.581181184014819330 ) ) ;
#11973 = ORIENTED_EDGE ( 'NONE', *, *, #11067, .T. ) ;
#11974 = CARTESIAN_POINT ( 'NONE',  ( -4.286401442266593698, 4.198423832313130433, 4.869383044678627925 ) ) ;
#11975 = CARTESIAN_POINT ( 'NONE',  ( 2.817313151351108047, 5.579000502529472882, 5.000000000000004441 ) ) ;
#11977 = ORIENTED_EDGE ( 'NONE', *, *, #12988, .T. ) ;
#11976 = LINE ( 'NONE', #47, #11572 ) ;
#11978 = CARTESIAN_POINT ( 'NONE',  ( 2.996920846510581438, -5.485395142346740194, 31.61441947245485196 ) ) ;
#11979 = VECTOR ( 'NONE', #12994, 1000.000000000000000 ) ;
#11980 = CARTESIAN_POINT ( 'NONE',  ( 2.583669522491375936, 226.7981340924959852, 5.880482682298685759 ) ) ;
#11981 = ORIENTED_EDGE ( 'NONE', *, *, #4036, .F. ) ;
#11982 = CARTESIAN_POINT ( 'NONE',  ( -4.267838854167198548, 4.217593933790310778, 11.23760108194401042 ) ) ;
#11983 = CARTESIAN_POINT ( 'NONE',  ( 2.066987300000000083, -0.8561741729129449530, -0.5999999989075250895 ) ) ;
#11984 = CARTESIAN_POINT ( 'NONE',  ( -2.799739712504301092, 226.9429308982220164, 6.307020443959882705 ) ) ;
#11985 =( NAMED_UNIT ( * ) PLANE_ANGLE_UNIT ( ) SI_UNIT ( $, .RADIAN. ) );
#11986 = CARTESIAN_POINT ( 'NONE',  ( 2.031800923367348393E-13, -6.250000000000000888, 23.49999999999999289 ) ) ;
#11987 = CARTESIAN_POINT ( 'NONE',  ( 1.035533905932737753, 186.4800000002185243, 4.500000000000000888 ) ) ;
#11988 = LINE ( 'NONE', #4844, #8590 ) ;
#11989 = CARTESIAN_POINT ( 'NONE',  ( 1.214181464861975757, 227.7437454098885041, 5.499312984720448938 ) ) ;
#11990 = CARTESIAN_POINT ( 'NONE',  ( 6.143143148203048298, 1.154591847827755702, 10.88603820591926841 ) ) ;
#11991 = CARTESIAN_POINT ( 'NONE',  ( 2.066987299999999639, 0.8561741729129456191, 1.100000001092475088 ) ) ;
#11992 = AXIS2_PLACEMENT_3D ( 'NONE', #3651, #2135, #9635 ) ;
#11993 = PLANE ( 'NONE',  #4159 ) ;
#11994 = ORIENTED_EDGE ( 'NONE', *, *, #10999, .T. ) ;
#11995 = CARTESIAN_POINT ( 'NONE',  ( -1.461580736456473906, 187.1499999989075320, 8.461580736456474128 ) ) ;
#11996 = PRODUCT_DEFINITION_SHAPE ( 'NONE', 'NONE',  #15747 ) ;
#11997 = CARTESIAN_POINT ( 'NONE',  ( -2.066987300000000527, 187.0499999989075093, 7.000000000000000000 ) ) ;
#11998 = CARTESIAN_POINT ( 'NONE',  ( -3.459447313391845746, -5.206669755180986847, 12.47400098023328674 ) ) ;
#11999 = VERTEX_POINT ( 'NONE', #7945 ) ;
#12000 = CARTESIAN_POINT ( 'NONE',  ( -2.692215568229910705, -5.362327947133556982, 24.23770962164066844 ) ) ;
#12001 = CARTESIAN_POINT ( 'NONE',  ( 0.5043776560899378980, -6.230795654995822552, 25.37337476296011118 ) ) ;
#12002 = CIRCLE ( 'NONE', #11247, 12.50000000000000533 ) ;
#12003 = LINE ( 'NONE', #10972, #6716 ) ;
#12004 = FACE_OUTER_BOUND ( 'NONE', #9266, .T. ) ;
#12005 = CARTESIAN_POINT ( 'NONE',  ( 0.8561741729129460632, 188.0999999989074922, 9.066987300000000971 ) ) ;
#12006 = CARTESIAN_POINT ( 'NONE',  ( 2.848235266351056616, -5.281699484015630830, 30.38602261056917442 ) ) ;
#12007 = CARTESIAN_POINT ( 'NONE',  ( 2.500000000000000000, 3.061616997868383141E-16, -0.1999999978150501789 ) ) ;
#12008 = CARTESIAN_POINT ( 'NONE',  ( 0.000000000000000000, 184.0000000000000000, -3.000000000000000888 ) ) ;
#12009 = LINE ( 'NONE', #10904, #1858 ) ;
#12010 = CARTESIAN_POINT ( 'NONE',  ( 0.9740856415301060167, -6.173834621338590622, 30.73852653055532969 ) ) ;
#12011 = CARTESIAN_POINT ( 'NONE',  ( -5.770167736194707686, 2.404664418229138345, 10.62632671364005255 ) ) ;
#12012 = DIRECTION ( 'NONE',  ( 0.000000000000000000, 0.000000000000000000, -1.000000000000000000 ) ) ;
#12013 = ADVANCED_FACE ( 'NONE', ( #15033 ), #465, .F. ) ;
#12014 = VERTEX_POINT ( 'NONE', #11596 ) ;
#12015 = VECTOR ( 'NONE', #875, 1000.000000000000000 ) ;
#12016 = EDGE_CURVE ( 'NONE', #3268, #15268, #8999, .T. ) ;
#12017 = ORIENTED_EDGE ( 'NONE', *, *, #4055, .F. ) ;
#12018 = B_SPLINE_CURVE_WITH_KNOTS ( 'NONE', 3,
 ( #12603, #13486, #1625, #2750, #6503, #11258, #6577, #2589, #11101, #8890, #123, #14688, #279, #3777, #14769, #2831, #7678, #12527 ),
 .UNSPECIFIED., .F., .F.,
 ( 4, 2, 2, 2, 2, 2, 2, 2, 4 ),
 ( 0.000000000000000000, 0.0003914898357794944594, 0.0007829796715589889189, 0.001174469507338483324, 0.001565959343117977838, 0.001957449178897472351, 0.002348939014676967516, 0.002740428850456463113, 0.003131918686235958278 ),
 .UNSPECIFIED. ) ;
#12019 = ORIENTED_EDGE ( 'NONE', *, *, #10132, .T. ) ;
#12020 = CARTESIAN_POINT ( 'NONE',  ( -5.317509234263959605, 2.779225709350992002, 31.00000000000000000 ) ) ;
#12021 = ORIENTED_EDGE ( 'NONE', *, *, #10846, .F. ) ;
#12022 = CARTESIAN_POINT ( 'NONE',  ( -0.8561741729129455081, 2.066987299999999639, 1.100000001092475088 ) ) ;
#12023 = CARTESIAN_POINT ( 'NONE',  ( -5.859221468178942516, -2.178708437343244597, 12.47408542334169113 ) ) ;
#12024 = FACE_OUTER_BOUND ( 'NONE', #1548, .T. ) ;
#12025 = CARTESIAN_POINT ( 'NONE',  ( -1.461580736456473462, 186.5499999989075093, 8.461580736456472351 ) ) ;
#12026 = CIRCLE ( 'NONE', #7203, 7.000000000000000000 ) ;
#12027 = CARTESIAN_POINT ( 'NONE',  ( 1.035533905932737531, 2.500000000000000444, -1.743000000021849960 ) ) ;
#12028 = DIRECTION ( 'NONE',  ( -0.9510565162951544194, 0.3090169943749447312, 0.000000000000000000 ) ) ;
#12029 = EDGE_CURVE ( 'NONE', #5008, #15704, #10683, .T. ) ;
#12030 = CARTESIAN_POINT ( 'NONE',  ( -2.066987299999999639, 0.000000000000000000, 2.250000001092474999 ) ) ;
#12031 = DIRECTION ( 'NONE',  ( 0.000000000000000000, 0.000000000000000000, 1.000000000000000000 ) ) ;
#12032 = CARTESIAN_POINT ( 'NONE',  ( 1.458867243353906273, 226.4466662005724800, 4.844797864602860216 ) ) ;
#12033 = DIRECTION ( 'NONE',  ( -1.000000000000000000, 0.000000000000000000, 0.000000000000000000 ) ) ;
#12034 = ORIENTED_EDGE ( 'NONE', *, *, #7108, .T. ) ;
#12035 = VERTEX_POINT ( 'NONE', #12478 ) ;
#12036 = EDGE_CURVE ( 'NONE', #9644, #3914, #543, .T. ) ;
#12037 = DIRECTION ( 'NONE',  ( -1.049359643968190670E-17, -1.165734175856414170E-15, 1.000000000000000000 ) ) ;
#12038 = ORIENTED_EDGE ( 'NONE', *, *, #3989, .F. ) ;
#12039 = CIRCLE ( 'NONE', #3901, 4.000000000000002665 ) ;
#12040 = ORIENTED_EDGE ( 'NONE', *, *, #7132, .T. ) ;
#12041 = CARTESIAN_POINT ( 'NONE',  ( 0.5042675786779335922, 6.230788509548837339, 31.87331068310448501 ) ) ;
#12042 = CARTESIAN_POINT ( 'NONE',  ( -4.435347140101157493, -4.403429997944390273, 24.36936067245787285 ) ) ;
#12043 = CARTESIAN_POINT ( 'NONE',  ( -2.692693252389695147, -5.362085866495053921, 24.76382603205594535 ) ) ;
#12044 = CARTESIAN_POINT ( 'NONE',  ( -5.903843691985217745, -2.055287728870688113, 32.00004906876532118 ) ) ;
#12045 = CARTESIAN_POINT ( 'NONE',  ( 4.005998022989810892, 4.467726698309398614, 25.29931806258175087 ) ) ;
#12046 = DIRECTION ( 'NONE',  ( -1.000000000000000000, 0.000000000000000000, 0.000000000000000000 ) ) ;
#12047 = CARTESIAN_POINT ( 'NONE',  ( 0.000000000000000000, 182.0000000000000000, -12.49999999999999822 ) ) ;
#12048 = CARTESIAN_POINT ( 'NONE',  ( 5.746619684944259454, 1.730157667110885367, 29.99995067926688108 ) ) ;
#12049 = CARTESIAN_POINT ( 'NONE',  ( 2.031800923283433283E-13, -6.000000000000000888, 23.49999999999999289 ) ) ;
#12050 = DIRECTION ( 'NONE',  ( -1.000000000000000000, 0.000000000000000000, 0.000000000000000000 ) ) ;
#12051 = CARTESIAN_POINT ( 'NONE',  ( -1.035533905932739751, 187.6499999978150584, 9.500000000000003553 ) ) ;
#12052 = CARTESIAN_POINT ( 'NONE',  ( 0.09803033623910094307, 226.3251703050289336, 4.486637493502143137 ) ) ;
#12053 = DIRECTION ( 'NONE',  ( 0.000000000000000000, 0.000000000000000000, 1.000000000000000000 ) ) ;
#12054 = EDGE_CURVE ( 'NONE', #14650, #28, #9742, .T. ) ;
#12055 = CARTESIAN_POINT ( 'NONE',  ( 5.621197618055683520, 2.101623592078498692, 31.97398020122239259 ) ) ;
#12056 = EDGE_LOOP ( 'NONE', ( #5287, #13913 ) ) ;
#12057 = CARTESIAN_POINT ( 'NONE',  ( -2.940898392866930777E-15, 228.9118723800512498, 8.872930300147352511 ) ) ;
#12058 = CARTESIAN_POINT ( 'NONE',  ( 0.6152055445546975587, -5.969096820685146909, 12.29904968670265930 ) ) ;
#12060 = EDGE_LOOP ( 'NONE', ( #2472, #14504, #7468, #2230 ) ) ;
#12059 = CARTESIAN_POINT ( 'NONE',  ( -2.500000000000000000, 0.000000000000000000, -0.7000000000000000666 ) ) ;
#12061 = CARTESIAN_POINT ( 'NONE',  ( 0.8499999999999896527, -0.3999999999999941380, -2.619018321873356037 ) ) ;
#12062 = DIRECTION ( 'NONE',  ( 0.000000000000000000, 0.000000000000000000, -1.000000000000000000 ) ) ;
#12063 = CARTESIAN_POINT ( 'NONE',  ( -4.196288036172476588, 4.288789315524806689, 10.99687951097621230 ) ) ;
#12064 = VECTOR ( 'NONE', #9094, 1000.000000000000114 ) ;
#12065 = CARTESIAN_POINT ( 'NONE',  ( -2.066987299999999639, 0.000000000000000000, -0.1499999989075253282 ) ) ;
#12066 = CARTESIAN_POINT ( 'NONE',  ( -2.947655337591893687, 227.4717885095516863, 7.864163344551670320 ) ) ;
#12067 = DIRECTION ( 'NONE',  ( 1.062480551894329776E-17, 2.775557561562888393E-16, -1.000000000000000000 ) ) ;
#12068 = CARTESIAN_POINT ( 'NONE',  ( 2.500000000000000444, 187.1800000002184845, 5.964466094067262247 ) ) ;
#12069 = CARTESIAN_POINT ( 'NONE',  ( 2.500000000000000444, -1.035533905932737309, -0.3500000000000000333 ) ) ;
#12070 = APPLICATION_CONTEXT ( 'automotive_design' ) ;
#12071 = CARTESIAN_POINT ( 'NONE',  ( -0.5154556838971166011, 227.6308307018634025, 5.173208867712369319 ) ) ;
#12072 = CARTESIAN_POINT ( 'NONE',  ( 1.050562149602352946, 228.8138732705275231, 8.589903282340008772 ) ) ;
#12073 = CARTESIAN_POINT ( 'NONE',  ( -2.066987299999999639, 0.000000000000000000, 1.450000001092474955 ) ) ;
#12074 = CARTESIAN_POINT ( 'NONE',  ( 0.8730424326981129912, 5.936362132114460621, 30.49500690218564358 ) ) ;
#12075 = ORIENTED_EDGE ( 'NONE', *, *, #14649, .F. ) ;
#12076 = CARTESIAN_POINT ( 'NONE',  ( -2.066987300000001415, 187.0999999989075206, 7.856174172912944620 ) ) ;
#12077 = CARTESIAN_POINT ( 'NONE',  ( 2.066987300000000527, 185.8499999989074922, 7.000000000000000000 ) ) ;
#12078 = CARTESIAN_POINT ( 'NONE',  ( -3.255013540813633366, -5.336859797930840976, 12.37381964045070859 ) ) ;
#12079 = ORIENTED_EDGE ( 'NONE', *, *, #13470, .T. ) ;
#12080 = CARTESIAN_POINT ( 'NONE',  ( 0.000000000000000000, 22.00000000000000000, 0.000000000000000000 ) ) ;
#12081 = CARTESIAN_POINT ( 'NONE',  ( -2.735911510694367108E-17, -3.993630376939310903E-16, 2.575022672948154234 ) ) ;
#12082 =( NAMED_UNIT ( * ) SI_UNIT ( $, .STERADIAN. ) SOLID_ANGLE_UNIT ( ) );
#12083 = CARTESIAN_POINT ( 'NONE',  ( -7.490007020835684592, -2.433650805992431110, 11.49999999999998224 ) ) ;
#12084 = CARTESIAN_POINT ( 'NONE',  ( -2.321326423937577488, 189.0000000000000000, 7.936319443449496802 ) ) ;
#12085 = CARTESIAN_POINT ( 'NONE',  ( 2.692143549875279707, 5.362363179736537866, 18.26194324003145653 ) ) ;
#12086 = CARTESIAN_POINT ( 'NONE',  ( 0.9085682364751954676, 189.0000000000368345, 9.333306381950002617 ) ) ;
#12087 = FACE_OUTER_BOUND ( 'NONE', #8769, .T. ) ;
#12088 = CARTESIAN_POINT ( 'NONE',  ( -3.000000000000000444, -1.732050807568878081, -2.500000000000000000 ) ) ;
#12089 = CARTESIAN_POINT ( 'NONE',  ( -5.375763363753442547, 2.665284979407548160, 10.99610204984015560 ) ) ;
#12090 = CARTESIAN_POINT ( 'NONE',  ( -5.570722351696268504, 2.834100162821960645, 11.23809786915986741 ) ) ;
#12091 = CARTESIAN_POINT ( 'NONE',  ( -5.903119516422487223, 1.077859910107424879, 30.38480617551147844 ) ) ;
#12092 = EDGE_CURVE ( 'NONE', #6866, #1061, #8004, .T. ) ;
#12093 = EDGE_LOOP ( 'NONE', ( #1684, #14206, #11845, #13308 ) ) ;
#12094 = EDGE_LOOP ( 'NONE', ( #14768, #12413 ) ) ;
#12095 = ORIENTED_EDGE ( 'NONE', *, *, #6399, .F. ) ;
#12096 = CARTESIAN_POINT ( 'NONE',  ( 0.2612504972992927277, 227.6131741670932342, 5.122215788231598843 ) ) ;
#12097 = VERTEX_POINT ( 'NONE', #7153 ) ;
#12098 = CARTESIAN_POINT ( 'NONE',  ( -1.530808498934191571E-16, 2.500000000000000000, -2.399999997815050801 ) ) ;
#12099 = CARTESIAN_POINT ( 'NONE',  ( 0.1306171417088619613, 6.000000000000000000, 4.000000000000004441 ) ) ;
#12100 = FACE_OUTER_BOUND ( 'NONE', #12, .T. ) ;
#12101 = CARTESIAN_POINT ( 'NONE',  ( 2.066987299999999639, 186.7999999989074809, 7.856174172912946396 ) ) ;
#12102 = CARTESIAN_POINT ( 'NONE',  ( 1.767766952966369320, -1.767766952966368654, 0.3999999999999997446 ) ) ;
#12103 = CARTESIAN_POINT ( 'NONE',  ( 5.558508435838229289, -2.857531096718853192, 5.000000000000004441 ) ) ;
#12104 = CONTEXT_DEPENDENT_SHAPE_REPRESENTATION ( #14107, #2075 ) ;
#12105 = CARTESIAN_POINT ( 'NONE',  ( 0.8561741729129463963, -2.066987299999999195, 1.700000001092474733 ) ) ;
#12106 = CARTESIAN_POINT ( 'NONE',  ( -5.131373506000769247, 7.062729720843990755, 11.49999999999998224 ) ) ;
#12107 = CARTESIAN_POINT ( 'NONE',  ( -2.976076845141470972, 227.1639356932526539, 6.957862568523350610 ) ) ;
#12108 = AXIS2_PLACEMENT_3D ( 'NONE', #11501, #5551, #12618 ) ;
#12109 = CARTESIAN_POINT ( 'NONE',  ( 6.176542424588105540, 0.9554180641286316167, 5.000000000000004441 ) ) ;
#12110 = VERTEX_POINT ( 'NONE', #6921 ) ;
#12111 = ORIENTED_EDGE ( 'NONE', *, *, #8593, .T. ) ;
#12112 = CARTESIAN_POINT ( 'NONE',  ( 1.767766952966368432, 188.5999999978150470, 8.767766952966368876 ) ) ;
#12113 = ORIENTED_EDGE ( 'NONE', *, *, #1472, .T. ) ;
#12114 = ORIENTED_EDGE ( 'NONE', *, *, #677, .T. ) ;
#12115 = CARTESIAN_POINT ( 'NONE',  ( -6.155854678529453672, 1.081900940642229081, 25.00425949503011225 ) ) ;
#12116 = EDGE_CURVE ( 'NONE', #10806, #10812, #1940, .T. ) ;
#12117 = CARTESIAN_POINT ( 'NONE',  ( -4.152999119458068655, -4.671604476854271049, 23.69973484982322276 ) ) ;
#12118 = CARTESIAN_POINT ( 'NONE',  ( 6.176542424588138402, 0.9554180641284283348, 24.36936067245787996 ) ) ;
#12119 = ADVANCED_FACE ( 'NONE', ( #6996 ), #3397, .T. ) ;
#12120 = CARTESIAN_POINT ( 'NONE',  ( -6.176542424588101987, -0.9554180641286524889, 31.00000000000000000 ) ) ;
#12121 = VECTOR ( 'NONE', #9534, 1000.000000000000000 ) ;
#12122 = DIRECTION ( 'NONE',  ( -0.5877852522924685852, -0.8090169943749507819, 0.000000000000000000 ) ) ;
#12123 = CARTESIAN_POINT ( 'NONE',  ( -1.965116437629976787E-16, 189.6999999978150697, 4.500000000000000000 ) ) ;
#12124 = CARTESIAN_POINT ( 'NONE',  ( -2.817313151351249711, 5.579000502529400940, 11.49999999999998224 ) ) ;
#12125 = CARTESIAN_POINT ( 'NONE',  ( 0.8737888311111418060, -5.936248257219488345, 18.50344185141215192 ) ) ;
#12126 = CARTESIAN_POINT ( 'NONE',  ( -1.035533905932737975, 188.2500000000000000, 4.500000000000001776 ) ) ;
#12127 = ADVANCED_FACE ( 'NONE', ( #857, #13103, #10566, #8265, #4685, #1016, #5724, #4522, #9377, #11681, #11825, #932, #1967, #6844, #5798, #15347, #780, #10493, #10644, #1095, #12947, #15506, #2203, #9298, #4604, #5879 ), #3242, .F. ) ;
#12128 = DIRECTION ( 'NONE',  ( 0.000000000000000000, -1.000000000000000000, 0.000000000000000000 ) ) ;
#12129 = CARTESIAN_POINT ( 'NONE',  ( 1.035533905932737753, 188.8499999978150470, 4.500000000000000888 ) ) ;
#12130 = B_SPLINE_CURVE_WITH_KNOTS ( 'NONE', 3,
 ( #11350, #5320, #13575, #10165, #15020, #9932, #10012, #13812, #14783, #2684, #12619, #7536, #6360, #11197, #1716, #11427, #296, #3308 ),
 .UNSPECIFIED., .F., .F.,
 ( 4, 2, 2, 2, 2, 2, 2, 2, 4 ),
 ( 0.000000000000000000, 0.0003914357524127504129, 0.0007828715048255008259, 0.001174307257238251185, 0.001565743009651001652, 0.001957178762063751902, 0.002348614514476502369, 0.002740050266889252836, 0.003131486019302003303 ),
 .UNSPECIFIED. ) ;
#12131 = CARTESIAN_POINT ( 'NONE',  ( 2.733135974173155791, 227.6887743597950760, 8.502598298417593625 ) ) ;
#12132 = PRODUCT_DEFINITION_FORMATION_WITH_SPECIFIED_SOURCE ( 'ANY', '', #166, .NOT_KNOWN. ) ;
#12133 = CARTESIAN_POINT ( 'NONE',  ( -6.176542424588084224, -0.9554180641287668418, 18.13237410716305220 ) ) ;
#12134 = CARTESIAN_POINT ( 'NONE',  ( -1.585779675826979984, 189.4204380473234721, 4.440511949549013515 ) ) ;
#12135 = VERTEX_POINT ( 'NONE', #3478 ) ;
#12136 = CARTESIAN_POINT ( 'NONE',  ( -5.317509234263939177, 2.779225709351033302, 11.49999999999998224 ) ) ;
#12137 = DIRECTION ( 'NONE',  ( 0.9510565162951500895, 0.3090169943749582204, 0.000000000000000000 ) ) ;
#12139 = VERTEX_POINT ( 'NONE', #8348 ) ;
#12138 = CARTESIAN_POINT ( 'NONE',  ( 5.487097279078493983, 2.429065649168680618, 25.29952054102716019 ) ) ;
#12140 = CARTESIAN_POINT ( 'NONE',  ( 0.04931887323393824990, -0.3999999999999923617, 2.539017587791714714 ) ) ;
#12141 = DIRECTION ( 'NONE',  ( -0.3090169943749446202, -0.9510565162951544194, 0.000000000000000000 ) ) ;
#12142 = VECTOR ( 'NONE', #4535, 1000.000000000000000 ) ;
#12143 = CARTESIAN_POINT ( 'NONE',  ( -4.142620314836410245, 4.341347824677476375, 10.88557478428060499 ) ) ;
#12144 = AXIS2_PLACEMENT_3D ( 'NONE', #15339, #2117, #6757 ) ;
#12145 = CARTESIAN_POINT ( 'NONE',  ( -2.066987299999999195, -0.8561741729129466183, -0.09999999890752520049 ) ) ;
#12146 = CARTESIAN_POINT ( 'NONE',  ( -4.290821322214536160, 4.545321419741401137, 23.88558052754514804 ) ) ;
#12147 = FACE_OUTER_BOUND ( 'NONE', #12093, .T. ) ;
#12148 = CARTESIAN_POINT ( 'NONE',  ( 1.767766952966369098, 186.4300000002185129, 5.232233047033630235 ) ) ;
#12149 = FACE_OUTER_BOUND ( 'NONE', #9342, .T. ) ;
#12150 = CARTESIAN_POINT ( 'NONE',  ( 1.990661649217015494, 228.2715988311494471, 7.023783772108481038 ) ) ;
#12151 = CARTESIAN_POINT ( 'NONE',  ( -0.8561741729129458411, -2.066987299999999195, 1.600000001092474866 ) ) ;
#12152 = CARTESIAN_POINT ( 'NONE',  ( 2.999999999999999556, 1.732050807568877859, -2.500000000000000000 ) ) ;
#12153 = ORIENTED_EDGE ( 'NONE', *, *, #10697, .F. ) ;
#12154 = CARTESIAN_POINT ( 'NONE',  ( -2.066987300000001415, 188.5999999989074922, 6.143825827087054492 ) ) ;
#12155 = AXIS2_PLACEMENT_3D ( 'NONE', #10554, #2267, #9768 ) ;
#12156 = CARTESIAN_POINT ( 'NONE',  ( 0.000000000000000000, 186.0499999989075093, 4.933012699999999029 ) ) ;
#12157 = CARTESIAN_POINT ( 'NONE',  ( 0.000000000000000000, 0.000000000000000000, 2.000000000000001776 ) ) ;
#12158 = EDGE_LOOP ( 'NONE', ( #8864, #10556 ) ) ;
#12159 = SURFACE_STYLE_FILL_AREA ( #3724 ) ;
#12160 = CARTESIAN_POINT ( 'NONE',  ( -5.317509234263835260, -2.779225709351231366, 24.49999999999999289 ) ) ;
#12161 = EDGE_CURVE ( 'NONE', #7643, #14650, #13187, .T. ) ;
#12162 = CARTESIAN_POINT ( 'NONE',  ( 1.354942164753511828E-13, -6.250000000000000888, 16.99999999999998579 ) ) ;
#12163 = CARTESIAN_POINT ( 'NONE',  ( 0.000000000000000000, 222.7460571280668091, 12.08513476933103625 ) ) ;
#12164 = CARTESIAN_POINT ( 'NONE',  ( 2.066987300000000083, 189.0999999989075206, 6.143825827087054492 ) ) ;
#12165 = AXIS2_PLACEMENT_3D ( 'NONE', #2499, #984, #7356 ) ;
#12166 = CARTESIAN_POINT ( 'NONE',  ( 4.267558728637157905, -4.217879122113839863, 18.26382603205596311 ) ) ;
#12167 = CARTESIAN_POINT ( 'NONE',  ( 1.767766952966369320, -1.767766952966368654, -2.699999997815051067 ) ) ;
#12168 = AXIS2_PLACEMENT_3D ( 'NONE', #12488, #6467, #13838 ) ;
#12169 = DIRECTION ( 'NONE',  ( -0.000000000000000000, 1.000000000000000000, -0.000000000000000000 ) ) ;
#12170 = DIRECTION ( 'NONE',  ( -0.8660254037844400399, 0.000000000000000000, 0.4999999999999975020 ) ) ;
#12171 = CARTESIAN_POINT ( 'NONE',  ( -0.6144300524832365662, -6.220417338033064070, 17.20033372175933195 ) ) ;
#12172 = CARTESIAN_POINT ( 'NONE',  ( 1.500000000000000000, 9.750000000000003553, 2.000000000000001776 ) ) ;
#12173 = CARTESIAN_POINT ( 'NONE',  ( -5.421010862427522170E-17, 187.4000000000000057, 4.500000000000000000 ) ) ;
#12174 = VERTEX_POINT ( 'NONE', #135 ) ;
#12175 = EDGE_LOOP ( 'NONE', ( #3117, #746 ) ) ;
#12176 = VECTOR ( 'NONE', #2659, 1000.000000000000000 ) ;
#12177 = ORIENTED_EDGE ( 'NONE', *, *, #2206, .T. ) ;
#12178 = CARTESIAN_POINT ( 'NONE',  ( -4.005361199355159663, 4.468319061418626781, 25.30022217383879024 ) ) ;
#12179 = ORIENTED_EDGE ( 'NONE', *, *, #4196, .T. ) ;
#12180 = CARTESIAN_POINT ( 'NONE',  ( -1.530808498934191571E-16, 2.500000000000000000, -1.599999997815050534 ) ) ;
#12181 = DIRECTION ( 'NONE',  ( 0.000000000000000000, 1.000000000000000000, 0.000000000000000000 ) ) ;
#12182 = DIRECTION ( 'NONE',  ( -0.3090169943749584980, 0.9510565162951498674, 0.000000000000000000 ) ) ;
#12183 = CARTESIAN_POINT ( 'NONE',  ( 0.8561741729129458411, 188.2999999989075093, 9.066987299999999195 ) ) ;
#12184 = CARTESIAN_POINT ( 'NONE',  ( -2.500000000000000000, 0.000000000000000000, 2.500000000000000000 ) ) ;
#12185 = CARTESIAN_POINT ( 'NONE',  ( -5.931734679891455642, 0.9039278060243561841, 31.26382603205594179 ) ) ;
#12186 = CARTESIAN_POINT ( 'NONE',  ( -5.770167736194620645, -2.404664418229350620, 25.37367328635991726 ) ) ;
#12187 = CARTESIAN_POINT ( 'NONE',  ( 3.796994071234844259E-16, -2.066987299999999639, -1.749999998907525223 ) ) ;
#12188 = CARTESIAN_POINT ( 'NONE',  ( 0.000000000000000000, 184.0000000000000000, 7.000000000000000000 ) ) ;
#12189 = CARTESIAN_POINT ( 'NONE',  ( -2.898051746902431614, 227.0396595591786308, 6.591911377507474690 ) ) ;
#12190 = CARTESIAN_POINT ( 'NONE',  ( 5.859155363331360888, 2.178872204145034797, 5.974000980233302727 ) ) ;
#12191 = VERTEX_POINT ( 'NONE', #13573 ) ;
#12192 = VERTEX_POINT ( 'NONE', #12302 ) ;
#12193 = VERTEX_POINT ( 'NONE', #2682 ) ;
#12194 = ORIENTED_EDGE ( 'NONE', *, *, #7405, .F. ) ;
#12195 = CARTESIAN_POINT ( 'NONE',  ( 1.038438454217461615, 189.0000000000000284, 9.278652157609089457 ) ) ;
#12196 = AXIS2_PLACEMENT_3D ( 'NONE', #8720, #6179, #9909 ) ;
#12197 = CARTESIAN_POINT ( 'NONE',  ( 6.123233995736766282E-16, -6.250000000000000888, 6.000000000000005329 ) ) ;
#12198 = CARTESIAN_POINT ( 'NONE',  ( -6.176542424588100211, -0.9554180641286524889, 31.13237410716304510 ) ) ;
#12199 = UNCERTAINTY_MEASURE_WITH_UNIT (LENGTH_MEASURE( 1.000000000000000082E-05 ), #12535, 'distance_accuracy_value', 'NONE');
#12200 = CARTESIAN_POINT ( 'NONE',  ( -2.500000000000000444, 184.0000000000000000, 7.000000000000000000 ) ) ;
#12201 = FACE_BOUND ( 'NONE', #9878, .T. ) ;
#12203 = DIRECTION ( 'NONE',  ( 1.000000000000000000, 0.000000000000000000, 0.000000000000000000 ) ) ;
#12202 = B_SPLINE_CURVE_WITH_KNOTS ( 'NONE', 3,
 ( #155, #3964, #1188, #2703, #6061, #7553, #1267, #2466, #3655, #5019, #12401, #9874, #8532, #13361, #9796, #1501, #14727, #11211 ),
 .UNSPECIFIED., .F., .F.,
 ( 4, 2, 2, 2, 2, 2, 2, 2, 4 ),
 ( 0.003131486019301978150, 0.003522824630466687024, 0.003914163241631395465, 0.004305501852796104340, 0.004696840463960812347, 0.005088179075125520354, 0.005479517686290228361, 0.005870856297454936368, 0.006262194908619644375 ),
 .UNSPECIFIED. ) ;
#12204 = CARTESIAN_POINT ( 'NONE',  ( 0.000000000000000000, 22.00000000000000000, 0.000000000000000000 ) ) ;
#12205 = FACE_OUTER_BOUND ( 'NONE', #104, .T. ) ;
#12206 = DIRECTION ( 'NONE',  ( -1.000000000000000000, 0.000000000000000000, 0.000000000000000000 ) ) ;
#12207 = CARTESIAN_POINT ( 'NONE',  ( -1.767766952966369765, 189.1999999978150697, 8.767766952966368876 ) ) ;
#12208 = CARTESIAN_POINT ( 'NONE',  ( 2.438651006298347301, 227.8520175407923034, 8.982830694042164055 ) ) ;
#12209 = CARTESIAN_POINT ( 'NONE',  ( 5.915699123067165388, 1.003533581835513999, 10.99610204984015915 ) ) ;
#12210 = ADVANCED_FACE ( 'NONE', ( #4763 ), #14378, .T. ) ;
#12211 = CARTESIAN_POINT ( 'NONE',  ( -2.928701478272802472, 189.8468539625636424, 7.998593929295510385 ) ) ;
#12212 = EDGE_LOOP ( 'NONE', ( #5829, #1602, #259, #9399 ) ) ;
#12213 = DIRECTION ( 'NONE',  ( -0.000000000000000000, 1.000000000000000000, -0.000000000000000000 ) ) ;
#12214 = DIRECTION ( 'NONE',  ( 0.000000000000000000, 0.000000000000000000, 1.000000000000000000 ) ) ;
#12215 = CARTESIAN_POINT ( 'NONE',  ( 5.665707375537499146, 1.979196487016603667, 25.50007961174476279 ) ) ;
#12216 = CARTESIAN_POINT ( 'NONE',  ( -4.435347140101057128, -4.403429997944487084, 11.49999999999998224 ) ) ;
#12217 = CARTESIAN_POINT ( 'NONE',  ( 0.1880867857842616064, 226.3251816858397092, 4.486670972203318009 ) ) ;
#12218 = CARTESIAN_POINT ( 'NONE',  ( -3.634089073485479382, 4.776071126502653641, 10.50007997643736601 ) ) ;
#12219 = EDGE_CURVE ( 'NONE', #7578, #5982, #12749, .T. ) ;
#12220 = CARTESIAN_POINT ( 'NONE',  ( -0.8561741729129455081, 2.066987299999999639, 0.5000000010924747773 ) ) ;
#12221 = CARTESIAN_POINT ( 'NONE',  ( 0.000000000000000000, 6.250000000000000888, 18.99999999999998934 ) ) ;
#12222 = DIRECTION ( 'NONE',  ( -6.123233995736766036E-17, 1.000000000000000000, 0.000000000000000000 ) ) ;
#12223 = CARTESIAN_POINT ( 'NONE',  ( 1.423015351387224570E-16, 184.1999999999999886, 4.500000000000000000 ) ) ;
#12224 = CYLINDRICAL_SURFACE ( 'NONE', #12620, 6.250000000000000888 ) ;
#12225 = ADVANCED_FACE ( 'NONE', ( #11717 ), #11560, .F. ) ;
#12226 = CARTESIAN_POINT ( 'NONE',  ( 0.4194150275617615775, 228.8973402254239033, 8.830960608724256033 ) ) ;
#12227 = CARTESIAN_POINT ( 'NONE',  ( 9.750000000000003553, 184.0000000000000000, 1.020968533498575461E-13 ) ) ;
#12228 = CARTESIAN_POINT ( 'NONE',  ( 5.903596343266304558, 2.055998103990562154, 17.00004921015705861 ) ) ;
#12229 = EDGE_LOOP ( 'NONE', ( #5668, #2650, #863, #7542 ) ) ;
#12230 = DIRECTION ( 'NONE',  ( 0.000000000000000000, 0.000000000000000000, 1.000000000000000000 ) ) ;
#12231 = CARTESIAN_POINT ( 'NONE',  ( -0.8561741729129458411, 187.6999999989075150, 4.933012699999999029 ) ) ;
#12232 = CARTESIAN_POINT ( 'NONE',  ( 5.409274167810704803, 2.597759609440538853, 23.88480617551148555 ) ) ;
#12234 = EDGE_LOOP ( 'NONE', ( #7877, #4290, #14487, #10573 ) ) ;
#12233 = CARTESIAN_POINT ( 'NONE',  ( -2.066987300000000083, 184.8499999989075206, 7.000000000000000000 ) ) ;
#12235 = CARTESIAN_POINT ( 'NONE',  ( -3.922672396097165670, -4.541739265057607611, 23.62635295315577011 ) ) ;
#12236 = CARTESIAN_POINT ( 'NONE',  ( 5.903347812666353001, -1.076697810262575272, 5.613977389430843346 ) ) ;
#12237 = EDGE_CURVE ( 'NONE', #13722, #10051, #10294, .T. ) ;
#12238 = CARTESIAN_POINT ( 'NONE',  ( 6.020822430078805354, -1.681351817312369823, 31.97408542334170889 ) ) ;
#12239 = CARTESIAN_POINT ( 'NONE',  ( -4.322356511625826236, 7.650514973136471220, 11.49999999999998224 ) ) ;
#12240 = CARTESIAN_POINT ( 'NONE',  ( -2.402303367210822049, 189.0000000000000284, 7.702985774066552160 ) ) ;
#12241 = CARTESIAN_POINT ( 'NONE',  ( 1.035533905932739085, -2.500000000000000000, 0.3500000000000000333 ) ) ;
#12242 = AXIS2_PLACEMENT_3D ( 'NONE', #4738, #2577, #12279 ) ;
#12243 = CARTESIAN_POINT ( 'NONE',  ( -2.500000000000000000, -1.035533905932739307, -2.949999997815051067 ) ) ;
#12244 = CARTESIAN_POINT ( 'NONE',  ( -0.5031281619707573816, -5.980084330432670292, 30.12602272744525678 ) ) ;
#12245 = CARTESIAN_POINT ( 'NONE',  ( 5.747343991580209810, -1.727858744772199584, 10.50007997643736424 ) ) ;
#12246 = CARTESIAN_POINT ( 'NONE',  ( -5.329907877631365309, 2.755840666746240508, 11.23805675996853104 ) ) ;
#12247 = CARTESIAN_POINT ( 'NONE',  ( 1.734723475976807094E-15, -0.001000000000000132727, 13.50000000000000000 ) ) ;
#12248 = DIRECTION ( 'NONE',  ( -1.000000000000000000, 0.000000000000000000, 0.000000000000000000 ) ) ;
#12249 = ORIENTED_EDGE ( 'NONE', *, *, #3894, .T. ) ;
#12250 = EDGE_CURVE ( 'NONE', #8636, #12288, #5530, .T. ) ;
#12251 = VERTEX_POINT ( 'NONE', #14101 ) ;
#12252 = PRODUCT_RELATED_PRODUCT_CATEGORY ( 'part', '', ( #2451 ) ) ;
#12253 = ORIENTED_EDGE ( 'NONE', *, *, #15184, .F. ) ;
#12254 = AXIS2_PLACEMENT_3D ( 'NONE', #7058, #7221, #3547 ) ;
#12255 = FACE_BOUND ( 'NONE', #640, .T. ) ;
#12256 = ORIENTED_EDGE ( 'NONE', *, *, #3115, .F. ) ;
#12257 = CARTESIAN_POINT ( 'NONE',  ( -1.461580736456472351, -1.461580736456473018, -1.849999998907525534 ) ) ;
#12258 = FACE_OUTER_BOUND ( 'NONE', #1915, .T. ) ;
#12259 = CARTESIAN_POINT ( 'NONE',  ( 0.000000000000000000, 19.99999999999999645, 0.000000000000000000 ) ) ;
#12260 = DIRECTION ( 'NONE',  ( -0.000000000000000000, -1.000000000000000000, -0.000000000000000000 ) ) ;
#12261 = CARTESIAN_POINT ( 'NONE',  ( -1.530808498934191571E-16, 2.500000000000000000, 2.299999999999999822 ) ) ;
#12262 = DIRECTION ( 'NONE',  ( -1.000000000000000000, 0.000000000000000000, 0.000000000000000000 ) ) ;
#12263 = ITEM_DEFINED_TRANSFORMATION ( 'NONE', 'NONE', #2801,  #14201 ) ;
#12264 = CARTESIAN_POINT ( 'NONE',  ( 3.312524433819824754, 5.004191858253972391, 5.974080527831012510 ) ) ;
#12265 = CARTESIAN_POINT ( 'NONE',  ( -2.066987299999999639, 0.000000000000000000, -1.149999998907525356 ) ) ;
#12266 = CIRCLE ( 'NONE', #7443, 5.000000000000000000 ) ;
#12267 = CYLINDRICAL_SURFACE ( 'NONE', #9884, 0.9999999999999998890 ) ;
#12268 = CARTESIAN_POINT ( 'NONE',  ( -2.668764612700158079, 227.7307401636093687, 8.626063590916809076 ) ) ;
#12269 = ORIENTED_EDGE ( 'NONE', *, *, #4732, .F. ) ;
#12270 = ORIENTED_EDGE ( 'NONE', *, *, #5417, .F. ) ;
#12271 = ADVANCED_FACE ( 'NONE', ( #10456 ), #1931, .F. ) ;
#12272 = VERTEX_POINT ( 'NONE', #4567 ) ;
#12273 = CARTESIAN_POINT ( 'NONE',  ( 5.935543223013862502, -0.8771126767606430841, 31.00000000000000000 ) ) ;
#12274 = CARTESIAN_POINT ( 'NONE',  ( 4.435347140101058905, -4.403429997944484420, 31.00000000000000000 ) ) ;
#12275 = CARTESIAN_POINT ( 'NONE',  ( -0.9739805876847985600, -5.920636045238166112, 5.261713868144209272 ) ) ;
#12276 = AXIS2_PLACEMENT_3D ( 'NONE', #5430, #14817, #13608 ) ;
#12277 = CARTESIAN_POINT ( 'NONE',  ( 1.000049271338626644, -6.169473353325530596, 17.86969612704554322 ) ) ;
#12278 = CARTESIAN_POINT ( 'NONE',  ( 0.9737778612006245949, 5.920671847850506708, 11.23736375884651828 ) ) ;
#12279 = DIRECTION ( 'NONE',  ( -1.000000000000000000, 0.000000000000000000, 0.000000000000000000 ) ) ;
#12280 = CARTESIAN_POINT ( 'NONE',  ( -6.176542424588120639, 0.9554180641285460185, 5.000000000000004441 ) ) ;
#12281 = DIRECTION ( 'NONE',  ( 0.000000000000000000, -1.000000000000000000, 0.000000000000000000 ) ) ;
#12282 = DIRECTION ( 'NONE',  ( -0.02708880405685116718, 0.000000000000000000, 0.9996330310142664821 ) ) ;
#12283 = DIRECTION ( 'NONE',  ( 0.000000000000000000, -1.000000000000000000, 0.000000000000000000 ) ) ;
#12284 = CARTESIAN_POINT ( 'NONE',  ( -2.500000000000000444, 189.0499999978150356, 5.964466094067261359 ) ) ;
#12285 = CARTESIAN_POINT ( 'NONE',  ( 2.809728313654571430, 226.9499418402095046, 6.327683296853605199 ) ) ;
#12286 = AXIS2_PLACEMENT_3D ( 'NONE', #5676, #10524, #11855 ) ;
#12287 = CARTESIAN_POINT ( 'NONE',  ( -3.003665301663284826, 189.8729084552422535, 7.414818630636749397 ) ) ;
#12288 = VERTEX_POINT ( 'NONE', #6805 ) ;
#12289 = DIRECTION ( 'NONE',  ( 1.000000000000000000, 0.000000000000000000, 0.000000000000000000 ) ) ;
#12290 = CARTESIAN_POINT ( 'NONE',  ( 4.153663429050794775, -4.670992970568362601, 10.70066851092421878 ) ) ;
#12291 = CARTESIAN_POINT ( 'NONE',  ( 5.915755444410821795, 1.003187219519724893, 25.00312048902375395 ) ) ;
#12292 = CARTESIAN_POINT ( 'NONE',  ( 0.2638277032950948620, 5.995407492418031836, 25.47332055281517782 ) ) ;
#12293 = CARTESIAN_POINT ( 'NONE',  ( 2.104503138662575878, 226.6021308763587285, 5.302993367608996422 ) ) ;
#12294 = DIRECTION ( 'NONE',  ( -6.123233995736766036E-17, 1.000000000000000000, 0.000000000000000000 ) ) ;
#12295 = EDGE_CURVE ( 'NONE', #26, #1214, #8034, .T. ) ;
#12296 = CARTESIAN_POINT ( 'NONE',  ( 3.796994071234844259E-16, -2.066987299999999639, -2.349999998907525089 ) ) ;
#12297 = DIRECTION ( 'NONE',  ( -0.000000000000000000, 1.000000000000000000, -0.000000000000000000 ) ) ;
#12298 = CARTESIAN_POINT ( 'NONE',  ( 9.750000000000003553, -1.020968533498575335E-13, 0.000000000000000000 ) ) ;
#12299 =( BOUNDED_CURVE ( )  B_SPLINE_CURVE ( 2, ( #630, #4300, #15280, #9163, #7960, #12800, #11611, #12876, #1902, #13997, #4382, #6776, #9237, #12357, #1982, #13550, #1454, #10657, #10578, #4537, #14476, #946, #791, #15517, #4616, #8444, #15438, #3253, #8120, #14300, #4456, #8280, #9469, #13114, #15360, #9551, #10738, #2215, #3409, #7085, #10504, #9311, #14389, #1027, #11922, #2379, #13280, #9388, #5813, #4778, #3573, #14226, #11692, #5891, #3493, #15598, #14151, #15677, #12958, #13203, #4699, #8363, #3333, #8201, #5658, #2058, #6934, #11765, #867, #13037, #5734, #2134, #7006, #5972, #2297, #10816, #7167, #12005, #1108, #11837, #9633, #3728, #14554, #9716, #5168, #10974, #13586, #8527, #8754, #2461, #10899, #231, #2697, #2619, #150, #8606, #3808, #12164, #7246, #13356, #13440 ),
 .UNSPECIFIED., .F., .F. ) 
 B_SPLINE_CURVE_WITH_KNOTS ( ( 3, 2, 2, 2, 2, 2, 2, 2, 2, 2, 2, 2, 2, 2, 2, 2, 2, 2, 2, 2, 2, 2, 2, 2, 2, 2, 2, 2, 2, 2, 2, 2, 2, 2, 2, 2, 2, 2, 2, 2, 2, 2, 2, 2, 2, 2, 2, 2, 2, 2, 3 ),
 ( 0.000000000000000000, 0.01785714285714285615, 0.03571428571428571230, 0.05357142857142856845, 0.07142857142857142461, 0.08928571428571428770, 0.1071428571428571369, 0.1250000000000000000, 0.1428571428571428492, 0.1607142857142857262, 0.1785714285714285754, 0.1964285714285714246, 0.2142857142857142738, 0.2321428571428571508, 0.2500000000000000000, 0.2678571428571428492, 0.2857142857142856984, 0.3035714285714285476, 0.3214285714285714524, 0.3392857142857143016, 0.3571428571428571508, 0.3750000000000000000, 0.3928571428571428492, 0.4107142857142856984, 0.4285714285714285476, 0.4464285714285714524, 0.4642857142857143016, 0.4821428571428571508, 0.5000000000000000000, 0.5178571428571429047, 0.5357142857142856984, 0.5535714285714286031, 0.5714285714285713969, 0.5892857142857143016, 0.6071428571428570953, 0.6250000000000000000, 0.6428571428571429047, 0.6607142857142856984, 0.6785714285714286031, 0.6964285714285715079, 0.7142857142857143016, 0.7321428571428570953, 0.7500000000000000000, 0.7678571428571429047, 0.7857142857142856984, 0.8035714285714286031, 0.8214285714285713969, 0.8392857142857143016, 0.8571428571428570953, 0.8750000000000000000, 0.8928571428571429047 ),
 .UNSPECIFIED. ) 
 CURVE ( )  GEOMETRIC_REPRESENTATION_ITEM ( )  RATIONAL_B_SPLINE_CURVE ( ( 1.000000000000000000, 0.9238795325112867385, 1.000000000000000000, 0.9238795325112867385, 1.000000000000000000, 0.9238795325112867385, 1.000000000000000000, 0.9238795325112867385, 1.000000000000000000, 0.9238795325112867385, 1.000000000000000000, 0.9238795325112867385, 1.000000000000000000, 0.9238795325112867385, 1.000000000000000000, 0.9238795325112867385, 1.000000000000000000, 0.9238795325112867385, 1.000000000000000000, 0.9238795325112867385, 1.000000000000000000, 0.9238795325112867385, 1.000000000000000000, 0.9238795325112867385, 1.000000000000000000, 0.9238795325112867385, 1.000000000000000000, 0.9238795325112867385, 1.000000000000000000, 0.9238795325112867385, 1.000000000000000000, 0.9238795325112867385, 1.000000000000000000, 0.9238795325112867385, 1.000000000000000000, 0.9238795325112867385, 1.000000000000000000, 0.9238795325112867385, 1.000000000000000000, 0.9238795325112867385, 1.000000000000000000, 0.9238795325112867385, 1.000000000000000000, 0.9238795325112867385, 1.000000000000000000, 0.9238795325112867385, 1.000000000000000000, 0.9238795325112867385, 1.000000000000000000, 0.9238795325112867385, 1.000000000000000000, 0.9238795325112867385, 1.000000000000000000, 0.9238795325112867385, 1.000000000000000000, 0.9238795325112867385, 1.000000000000000000, 0.9238795325112867385, 1.000000000000000000, 0.9238795325112867385, 1.000000000000000000, 0.9238795325112867385, 1.000000000000000000, 0.9238795325112867385, 1.000000000000000000, 0.9238795325112867385, 1.000000000000000000, 0.9238795325112867385, 1.000000000000000000, 0.9238795325112867385, 1.000000000000000000, 0.9238795325112867385, 1.000000000000000000, 0.9238795325112867385, 1.000000000000000000, 0.9238795325112867385, 1.000000000000000000, 0.9238795325112867385, 1.000000000000000000, 0.9238795325112867385, 1.000000000000000000, 0.9238795325112867385, 1.000000000000000000, 0.9238795325112867385, 1.000000000000000000, 0.9238795325112867385, 1.000000000000000000, 0.9238795325112867385, 1.000000000000000000, 0.9238795325112867385, 1.000000000000000000, 0.9238795325112867385, 1.000000000000000000, 0.9238795325112867385, 1.000000000000000000, 0.9238795325112867385, 1.000000000000000000, 0.9238795325112867385, 1.000000000000000000, 0.9238795325112867385, 1.000000000000000000 ) ) 
 REPRESENTATION_ITEM ( '' )  );
#12300 = CARTESIAN_POINT ( 'NONE',  ( -3.388131789017201356E-18, 186.5300000002185072, 4.500000000000000000 ) ) ;
#12301 = FACE_OUTER_BOUND ( 'NONE', #4419, .T. ) ;
#12302 = CARTESIAN_POINT ( 'NONE',  ( 5.317509234263970264, -2.779225709350972906, 5.000000000000004441 ) ) ;
#12303 = FACE_OUTER_BOUND ( 'NONE', #11142, .T. ) ;
#12304 = CARTESIAN_POINT ( 'NONE',  ( 0.9999196734182850266, 5.916093360767511022, 30.86725955955067136 ) ) ;
#12305 = ORIENTED_EDGE ( 'NONE', *, *, #2535, .T. ) ;
#12306 = CARTESIAN_POINT ( 'NONE',  ( -2.066987299999999639, 0.000000000000000000, 0.4500000010924747329 ) ) ;
#12307 = CARTESIAN_POINT ( 'NONE',  ( -1.461580736456473684, 184.7499999989074979, 8.461580736456474128 ) ) ;
#12308 = B_SPLINE_CURVE_WITH_KNOTS ( 'NONE', 3,
 ( #15385, #4481, #3284, #6957, #11001, #14665, #5995, #2403, #3519, #13140, #8302, #15544, #9572, #13061, #9817, #2159, #14500, #8390 ),
 .UNSPECIFIED., .F., .F.,
 ( 4, 2, 2, 2, 2, 2, 2, 2, 4 ),
 ( 0.000000000000000000, 0.0003914357524127473230, 0.0007828715048254946459, 0.001174307257238241860, 0.001565743009650990376, 0.001957178762063739759, 0.002348614514476488925, 0.002740050266889238525, 0.003131486019301987691 ),
 .UNSPECIFIED. ) ;
#12309 = CARTESIAN_POINT ( 'NONE',  ( 7.000000000000006217, -4.163336342344337027E-16, 1.500000000000001776 ) ) ;
#12311 = EDGE_LOOP ( 'NONE', ( #15569, #11367, #1913, #6147 ) ) ;
#12310 = CARTESIAN_POINT ( 'NONE',  ( 1.461580736456472573, 185.9499999989075150, 8.461580736456474128 ) ) ;
#12312 = FACE_OUTER_BOUND ( 'NONE', #12774, .T. ) ;
#12313 = AXIS2_PLACEMENT_3D ( 'NONE', #14215, #4444, #12863 ) ;
#12314 = ADVANCED_FACE ( 'NONE', ( #2086 ), #6959, .T. ) ;
#12315 = CYLINDRICAL_SURFACE ( 'NONE', #15448, 1.000000000000000666 ) ;
#12316 = ADVANCED_FACE ( 'NONE', ( #8476 ), #11003, .F. ) ;
#12317 =( NAMED_UNIT ( * ) PLANE_ANGLE_UNIT ( ) SI_UNIT ( $, .RADIAN. ) );
#12318 = CARTESIAN_POINT ( 'NONE',  ( 3.659182332138577465E-16, 187.9952603975225713, 3.440894205938198613 ) ) ;
#12319 = CARTESIAN_POINT ( 'NONE',  ( -0.2693458344851792918, 189.0000000000000284, 9.494867214852071413 ) ) ;
#12320 = CARTESIAN_POINT ( 'NONE',  ( 5.329945432499706648, -2.755769831644989232, 24.76229037835931734 ) ) ;
#12321 = CARTESIAN_POINT ( 'NONE',  ( 0.4831378333609244180, 2.500000000000000000, -3.223327956010960449 ) ) ;
#12322 = DIRECTION ( 'NONE',  ( 1.000000000000000000, 0.000000000000000000, 0.000000000000000000 ) ) ;
#12323 = CARTESIAN_POINT ( 'NONE',  ( 1.340391840173529081, 189.7235632956260361, 10.07394016998248887 ) ) ;
#12324 = CARTESIAN_POINT ( 'NONE',  ( -0.7995524673974289120, -6.199337389817286770, 18.61453679452458232 ) ) ;
#12325 = CARTESIAN_POINT ( 'NONE',  ( 7.490007020835686369, -2.433650805992243260, 5.000000000000004441 ) ) ;
#12326 = CARTESIAN_POINT ( 'NONE',  ( 4.141923667210504867, 4.342011609040599573, 23.88438267301394191 ) ) ;
#12327 = B_SPLINE_CURVE_WITH_KNOTS ( 'NONE', 3,
 ( #9558, #2141, #10745, #8287, #6863, #12884, #4390, #14158, #1911, #14396, #6784, #3340, #10513, #2223, #3261, #5898, #1034, #11929 ),
 .UNSPECIFIED., .F., .F.,
 ( 4, 2, 2, 2, 2, 2, 2, 2, 4 ),
 ( 0.003131923598877003109, 0.003523316383094320450, 0.003914709167311637358, 0.004306101951528954266, 0.004697494735746271174, 0.005088887519963588082, 0.005480280304180905858, 0.005871673088398223633, 0.006263065872615540541 ),
 .UNSPECIFIED. ) ;
#12328 = ORIENTED_EDGE ( 'NONE', *, *, #7354, .F. ) ;
#12329 = CARTESIAN_POINT ( 'NONE',  ( 1.461580736456472795, 187.7499999989075263, 5.538419263543527649 ) ) ;
#12330 = ORIENTED_EDGE ( 'NONE', *, *, #10606, .F. ) ;
#12331 = EDGE_LOOP ( 'NONE', ( #1586, #9366 ) ) ;
#12332 = CARTESIAN_POINT ( 'NONE',  ( -5.375763363753348401, -2.665284979407742671, 25.00389795015983552 ) ) ;
#12333 = VERTEX_POINT ( 'NONE', #6080 ) ;
#12334 = CARTESIAN_POINT ( 'NONE',  ( -0.8561741729129455081, 2.066987299999999639, -0.4999999989075253337 ) ) ;
#12335 = VECTOR ( 'NONE', #3780, 1000.000000000000000 ) ;
#12336 = CARTESIAN_POINT ( 'NONE',  ( -1.084202172485504434E-16, 3.464101615137754830, -5.500000000000000000 ) ) ;
#12337 = CARTESIAN_POINT ( 'NONE',  ( -1.992790919479760392, 190.0169567515527262, 4.969246669617095158 ) ) ;
#12338 = CARTESIAN_POINT ( 'NONE',  ( 1.979652835806277785E-15, 2.000000000000000000, 11.50000000000000000 ) ) ;
#12340 = CARTESIAN_POINT ( 'NONE',  ( 2.500000000000000444, -1.035533905932737309, 0.4499999999999998446 ) ) ;
#12339 = B_SPLINE_CURVE_WITH_KNOTS ( 'NONE', 3,
 ( #12772, #10480, #1798, #6984, #15253, #11813, #4354, #1955, #9363, #14124, #9213, #14204, #917, #4431, #8012, #15410, #11506, #3157 ),
 .UNSPECIFIED., .F., .F.,
 ( 4, 2, 2, 2, 2, 2, 2, 2, 4 ),
 ( 0.003131486019301973813, 0.003522824630466682688, 0.003914163241631391128, 0.004305501852796100003, 0.004696840463960808877, 0.005088179075125516884, 0.005479517686290227493, 0.005870856297454936368, 0.006262194908619646110 ),
 .UNSPECIFIED. ) ;
#12341 = CARTESIAN_POINT ( 'NONE',  ( 5.616116467183635663, -2.743044348085595718, 4.495740504969914397 ) ) ;
#12342 = ITEM_DEFINED_TRANSFORMATION ( 'NONE', 'NONE', #2220,  #14201 ) ;
#12343 = CARTESIAN_POINT ( 'NONE',  ( 3.419318284370281180, -4.932111238568118949, 31.99992002356261267 ) ) ;
#12344 = CARTESIAN_POINT ( 'NONE',  ( 3.796994071234844259E-16, -2.066987299999999639, -0.7499999989075251117 ) ) ;
#12345 = DIRECTION ( 'NONE',  ( 0.000000000000000000, 1.000000000000000000, 0.000000000000000000 ) ) ;
#12346 = CARTESIAN_POINT ( 'NONE',  ( -2.440032737085090275, 227.8520529458832300, 8.982935890751354790 ) ) ;
#12347 = VERTEX_POINT ( 'NONE', #1209 ) ;
#12348 = ORIENTED_EDGE ( 'NONE', *, *, #15326, .T. ) ;
#12349 = EDGE_LOOP ( 'NONE', ( #4854, #8116, #10790, #13194 ) ) ;
#12350 = EDGE_CURVE ( 'NONE', #26, #3801, #4805, .T. ) ;
#12351 = CARTESIAN_POINT ( 'NONE',  ( 5.915755444410805808, -1.003187219519832585, 30.49687951097622118 ) ) ;
#12352 = CARTESIAN_POINT ( 'NONE',  ( 2.278945589504768776, 189.0000000000000568, 8.040059659319428675 ) ) ;
#12353 = CARTESIAN_POINT ( 'NONE',  ( 0.1306070469493385289, 6.250000000000000000, 4.000000000000004441 ) ) ;
#12354 = CARTESIAN_POINT ( 'NONE',  ( 13.50000000000000000, -0.001000000000000132727, 1.999999999999998668 ) ) ;
#12355 = CARTESIAN_POINT ( 'NONE',  ( 0.2638277032949492007, 5.995407492418038053, 12.47332055281516716 ) ) ;
#12356 = CARTESIAN_POINT ( 'NONE',  ( -1.035533905932739529, 186.0499999978150356, 9.500000000000003553 ) ) ;
#12357 = CARTESIAN_POINT ( 'NONE',  ( 0.8561741729129461742, 184.8999999989075320, 9.066987300000000971 ) ) ;
#12358 = ADVANCED_FACE ( 'NONE', ( #14668 ), #9575, .T. ) ;
#12359 = CARTESIAN_POINT ( 'NONE',  ( -5.558508435838226625, 2.857531096718854968, 5.130606907234993130 ) ) ;
#12360 = CARTESIAN_POINT ( 'NONE',  ( 0.9740807849838198917, -5.920620690450655310, 24.23850119700669126 ) ) ;
#12361 = DIRECTION ( 'NONE',  ( 1.000000000000000000, 0.000000000000000000, 0.000000000000000000 ) ) ;
#12362 = CARTESIAN_POINT ( 'NONE',  ( -2.500000000000000444, 187.5699999975965397, 7.000000000000000000 ) ) ;
#12363 = CARTESIAN_POINT ( 'NONE',  ( -1.990672364496464342, 228.2390692824501457, 6.929836580100483090 ) ) ;
#12364 = CARTESIAN_POINT ( 'NONE',  ( -2.995192278888715975, 227.2265329420484647, 7.142163989385624134 ) ) ;
#12365 = CARTESIAN_POINT ( 'NONE',  ( -2.324167314932467310, 189.0000000021436222, 7.935049049248011244 ) ) ;
#12366 = ORIENTED_EDGE ( 'NONE', *, *, #358, .T. ) ;
#12367 = CARTESIAN_POINT ( 'NONE',  ( -5.726307184802613470, 2.506131700382554950, 17.19973484982324408 ) ) ;
#12368 = APPLICATION_CONTEXT ( 'automotive_design' ) ;
#12369 = CARTESIAN_POINT ( 'NONE',  ( -5.570722351696208108, 2.834100162822084101, 24.23809786915987985 ) ) ;
#12370 = CARTESIAN_POINT ( 'NONE',  ( -0.1323736289504354180, 6.250000000000000888, 6.000000000000004441 ) ) ;
#12371 = CARTESIAN_POINT ( 'NONE',  ( 6.020822430078779597, 1.681351817312460861, 30.02591457665829111 ) ) ;
#12372 = CARTESIAN_POINT ( 'NONE',  ( 2.782695181561366304, 227.6502397201549570, 8.389219295768896245 ) ) ;
#12373 = CARTESIAN_POINT ( 'NONE',  ( -3.883588957979168477, -4.898466244119000557, 31.97377282875268989 ) ) ;
#12374 = CARTESIAN_POINT ( 'NONE',  ( 2.500000000000000444, 1.035533905932737975, 1.350000000000000089 ) ) ;
#12375 = CARTESIAN_POINT ( 'NONE',  ( -4.070863287254287144, 4.743975846881624214, 23.62694108445698760 ) ) ;
#12376 = ORIENTED_EDGE ( 'NONE', *, *, #13518, .F. ) ;
#12377 = CARTESIAN_POINT ( 'NONE',  ( -3.882673863916222601, -4.899192824800991275, 30.02591457665829466 ) ) ;
#12378 = CARTESIAN_POINT ( 'NONE',  ( 1.767766952966368432, 186.2999999999999829, 8.767766952966368876 ) ) ;
#12379 = CARTESIAN_POINT ( 'NONE',  ( 1.767766952966369320, -1.767766952966368654, -0.4000000000000001887 ) ) ;
#12380 = ADVANCED_BREP_SHAPE_REPRESENTATION ( '', ( #4943, #14201 ), #4042 ) ;
#12381 = CARTESIAN_POINT ( 'NONE',  ( 0.8212144138252523984, 228.8542370555972809, 8.706476195820313180 ) ) ;
#12382 = CARTESIAN_POINT ( 'NONE',  ( 3.796994071234844259E-16, -2.066987299999999639, -2.349999998907525089 ) ) ;
#12383 = CARTESIAN_POINT ( 'NONE',  ( 6.081590040723123813, -1.446205118472801754, 25.37367328635992081 ) ) ;
#12384 = CARTESIAN_POINT ( 'NONE',  ( 9.750000000000003553, -1.020968533498575335E-13, 2.000000000000001776 ) ) ;
#12385 = CARTESIAN_POINT ( 'NONE',  ( -2.066987300000000971, 188.6499999989075036, 7.000000000000000000 ) ) ;
#12386 = CARTESIAN_POINT ( 'NONE',  ( -3.827021247335478803E-16, 2.500000000000000000, -2.500000000000000000 ) ) ;
#12387 = AXIS2_PLACEMENT_3D ( 'NONE', #5321, #13576, #14860 ) ;
#12389 = VERTEX_POINT ( 'NONE', #10923 ) ;
#12388 = CARTESIAN_POINT ( 'NONE',  ( -1.461580736456473018, 186.3499999989075206, 5.538419263543527649 ) ) ;
#12390 = CARTESIAN_POINT ( 'NONE',  ( -4.152999119458038457, -4.671604476854300358, 17.19973484982324408 ) ) ;
#12391 =( REPRESENTATION_RELATIONSHIP ('NONE','NONE', #11191, #4596 ) REPRESENTATION_RELATIONSHIP_WITH_TRANSFORMATION ( #8779 )SHAPE_REPRESENTATION_RELATIONSHIP( ) );
#12392 = DIRECTION ( 'NONE',  ( -0.5877852522924685852, -0.8090169943749508930, 0.000000000000000000 ) ) ;
#12393 = CARTESIAN_POINT ( 'NONE',  ( 4.344313232727081697, -4.493553492990136178, 17.49563030319847101 ) ) ;
#12394 = CARTESIAN_POINT ( 'NONE',  ( -5.375763363753478075, 2.665284979407481547, 4.496102049840166259 ) ) ;
#12395 = CARTESIAN_POINT ( 'NONE',  ( -0.6156133477426046774, -6.220296490279947577, 12.29872387345510454 ) ) ;
#12396 = CARTESIAN_POINT ( 'NONE',  ( 2.668367453516506504, 5.373994336898192614, 17.99999999999998934 ) ) ;
#12397 = DIRECTION ( 'NONE',  ( -0.000000000000000000, 1.000000000000000000, -0.000000000000000000 ) ) ;
#12398 = FACE_OUTER_BOUND ( 'NONE', #3245, .T. ) ;
#12399 = CARTESIAN_POINT ( 'NONE',  ( 5.375913338529123564, -2.664979843780373336, 10.99571079637980553 ) ) ;
#12401 = CARTESIAN_POINT ( 'NONE',  ( -3.459447313391871059, 5.206669755180970860, 30.02599901976670438 ) ) ;
#12400 = AXIS2_PLACEMENT_3D ( 'NONE', #10441, #1763, #15294 ) ;
#12402 = CARTESIAN_POINT ( 'NONE',  ( 2.500000000000000444, 185.4999999978150527, 7.000000000000000000 ) ) ;
#12403 = CARTESIAN_POINT ( 'NONE',  ( -5.665308849928797130, -1.980336949702578009, 10.50007997643736424 ) ) ;
#12404 = EDGE_CURVE ( 'NONE', #786, #9805, #14416, .T. ) ;
#12405 = ORIENTED_EDGE ( 'NONE', *, *, #4301, .F. ) ;
#12406 = CARTESIAN_POINT ( 'NONE',  ( 1.461580736456472351, 187.5499999989075093, 8.461580736456474128 ) ) ;
#12407 = EDGE_CURVE ( 'NONE', #5925, #2012, #4202, .T. ) ;
#12408 = EDGE_LOOP ( 'NONE', ( #4549, #3718 ) ) ;
#12409 = CARTESIAN_POINT ( 'NONE',  ( -5.935543223013816316, -0.8771126767609508379, 24.49999999999999289 ) ) ;
#12410 = ORIENTED_EDGE ( 'NONE', *, *, #557, .F. ) ;
#12411 = DIRECTION ( 'NONE',  ( 0.000000000000000000, -0.000000000000000000, -1.000000000000000000 ) ) ;
#12412 = CARTESIAN_POINT ( 'NONE',  ( 4.435347140100866170, 4.403429997944679819, 24.49999999999999289 ) ) ;
#12413 = ORIENTED_EDGE ( 'NONE', *, *, #7306, .F. ) ;
#12414 = VECTOR ( 'NONE', #3781, 1000.000000000000000 ) ;
#12415 = CARTESIAN_POINT ( 'NONE',  ( 2.066987300000000083, -0.8561741729129449530, -0.7999999989075252671 ) ) ;
#12416 = CARTESIAN_POINT ( 'NONE',  ( -3.781065399485988188, 4.978303713186458701, 4.000082581897114409 ) ) ;
#12417 = CARTESIAN_POINT ( 'NONE',  ( -2.604939343947620500, 189.9599476955858393, 5.742039956245639232 ) ) ;
#12418 = DIRECTION ( 'NONE',  ( 0.5877852522924802425, -0.8090169943749422332, 0.000000000000000000 ) ) ;
#12419 = CARTESIAN_POINT ( 'NONE',  ( -1.767766952966368432, -1.767766952966369320, 0.2000000000000000944 ) ) ;
#12420 = CARTESIAN_POINT ( 'NONE',  ( -4.286401442266690509, 4.198423832313033621, 17.86938304467860306 ) ) ;
#12421 = CARTESIAN_POINT ( 'NONE',  ( 3.922288969639793343, 4.542045818322514528, 5.873784308702619583 ) ) ;
#12422 = CARTESIAN_POINT ( 'NONE',  ( -1.265664690411614835E-16, 2.066987299999999639, -0.3499999989075254225 ) ) ;
#12423 = CARTESIAN_POINT ( 'NONE',  ( 5.571002711501443549, -2.833546409886217976, 11.23620383159194525 ) ) ;
#12424 = CARTESIAN_POINT ( 'NONE',  ( -2.734462099041327310, 226.8914831935726966, 6.155496219900511434 ) ) ;
#12425 = EDGE_CURVE ( 'NONE', #8130, #159, #2243, .T. ) ;
#12426 = VERTEX_POINT ( 'NONE', #13142 ) ;
#12427 = STYLED_ITEM ( 'NONE', ( #1884 ), #1193 ) ;
#12428 = ORIENTED_EDGE ( 'NONE', *, *, #13727, .F. ) ;
#12429 = ORIENTED_EDGE ( 'NONE', *, *, #1166, .T. ) ;
#12430 = CARTESIAN_POINT ( 'NONE',  ( 0.9739805876849262356, 5.920636045238144796, 18.26171386814421638 ) ) ;
#12431 = CARTESIAN_POINT ( 'NONE',  ( 0.08806441522324243154, 188.9999999999999716, 9.502418536650717229 ) ) ;
#12432 = ORIENTED_EDGE ( 'NONE', *, *, #11126, .F. ) ;
#12433 = CARTESIAN_POINT ( 'NONE',  ( 2.500000000000000000, 188.7999999999999829, 7.000000000000000000 ) ) ;
#12434 = CARTESIAN_POINT ( 'NONE',  ( 0.9740807849836315979, -5.920620690450686396, 30.73850119700668415 ) ) ;
#12435 = CARTESIAN_POINT ( 'NONE',  ( -1.265664690411614835E-16, 2.066987299999999639, -2.749999998907525001 ) ) ;
#12436 = AXIS2_PLACEMENT_3D ( 'NONE', #348, #189, #3844 ) ;
#12437 = CARTESIAN_POINT ( 'NONE',  ( 0.3133709289838055301, -0.3999999999999906408, -2.571515392584351023 ) ) ;
#12438 = CARTESIAN_POINT ( 'NONE',  ( -1.767766952966369098, 185.7999999978150356, 5.232233047033630235 ) ) ;
#12439 = CYLINDRICAL_SURFACE ( 'NONE', #391, 20.00000000000000000 ) ;
#12440 = B_SPLINE_CURVE_WITH_KNOTS ( 'NONE', 3,
 ( #9652, #2314, #13298, #2560, #10832, #90, #15694, #14493, #10917, #6073, #8698, #3590, #14408, #3513, #9734, #15614, #3746, #4716 ),
 .UNSPECIFIED., .F., .F.,
 ( 4, 2, 2, 2, 2, 2, 2, 2, 4 ),
 ( 0.003131486019301973379, 0.003522824630466680519, 0.003914163241631388526, 0.004305501852796095666, 0.004696840463960802806, 0.005088179075125510813, 0.005479517686290218820, 0.005870856297454926827, 0.006262194908619634834 ),
 .UNSPECIFIED. ) ;
#12441 = DIRECTION ( 'NONE',  ( -1.000000000000000000, 3.326610055774637112E-18, 1.062480551894331163E-17 ) ) ;
#12442 = DIRECTION ( 'NONE',  ( 0.000000000000000000, -1.000000000000000000, 0.000000000000000000 ) ) ;
#12443 = CARTESIAN_POINT ( 'NONE',  ( 2.500000000000000444, 184.7699999975965568, 7.000000000000000000 ) ) ;
#12444 = CARTESIAN_POINT ( 'NONE',  ( 0.4220225674029139951, 227.6236908799334344, 5.152588654748359254 ) ) ;
#12445 = CARTESIAN_POINT ( 'NONE',  ( -1.501309217710235622, 226.4539600517547910, 4.866297710963618073 ) ) ;
#12446 = CARTESIAN_POINT ( 'NONE',  ( -2.260484549978974744, 188.9999999992296296, 8.078936515875282609 ) ) ;
#12447 = EDGE_CURVE ( 'NONE', #10051, #8233, #15621, .T. ) ;
#12448 = ORIENTED_EDGE ( 'NONE', *, *, #8473, .T. ) ;
#12449 = CARTESIAN_POINT ( 'NONE',  ( -5.915641100987826029, 1.003868594704782069, 12.00428920362018914 ) ) ;
#12450 = FACE_OUTER_BOUND ( 'NONE', #11774, .T. ) ;
#12451 = CARTESIAN_POINT ( 'NONE',  ( 1.734723475976807094E-15, 0.000000000000000000, 13.50000000000000000 ) ) ;
#12452 = CARTESIAN_POINT ( 'NONE',  ( 6.143143148203041193, 1.154591847827807882, 30.38603820591927374 ) ) ;
#12453 = CARTESIAN_POINT ( 'NONE',  ( 2.753714765446583446, 226.9066926092818051, 6.200293790039342667 ) ) ;
#12454 = EDGE_CURVE ( 'NONE', #7039, #7931, #4707, .T. ) ;
#12455 = CARTESIAN_POINT ( 'NONE',  ( -2.817313151351126255, -5.579000502529464001, 31.00000000000000000 ) ) ;
#12456 = CARTESIAN_POINT ( 'NONE',  ( 1.767766952966369320, -1.767766952966368654, 1.199999999999999956 ) ) ;
#12457 = CARTESIAN_POINT ( 'NONE',  ( 5.867109477881239599, -1.259218163100936927, 4.201117577520603774 ) ) ;
#12458 = CARTESIAN_POINT ( 'NONE',  ( -4.291255145204003973, -4.544933371694741098, 30.38603820591928439 ) ) ;
#12459 = CARTESIAN_POINT ( 'NONE',  ( 4.404571325722361763E-17, 185.7999999999999829, 4.500000000000000000 ) ) ;
#12460 = FACE_BOUND ( 'NONE', #8175, .T. ) ;
#12461 = CARTESIAN_POINT ( 'NONE',  ( 0.6422548253168780530, 227.6434438162357878, 5.209636261422765813 ) ) ;
#12462 = CARTESIAN_POINT ( 'NONE',  ( 0.8561741729129465073, -2.066987299999999195, -2.299999998907525267 ) ) ;
#12463 = CARTESIAN_POINT ( 'NONE',  ( 1.035533905932739085, -2.500000000000000000, -2.749999997815050445 ) ) ;
#12464 = CARTESIAN_POINT ( 'NONE',  ( 2.066987299999999639, 2.531329380823229670E-16, 0.05000000109247476621 ) ) ;
#12465 = CARTESIAN_POINT ( 'NONE',  ( -1.461580736456473240, 188.5499999989075093, 5.538419263543526760 ) ) ;
#12466 = CARTESIAN_POINT ( 'NONE',  ( -5.375763363753377710, -2.665284979407680943, 18.50389795015982841 ) ) ;
#12468 = VERTEX_POINT ( 'NONE', #2321 ) ;
#12467 = CARTESIAN_POINT ( 'NONE',  ( -6.098637220230962441E-17, 187.0499999989075093, 4.933012699999999029 ) ) ;
#12469 = VECTOR ( 'NONE', #6988, 1000.000000000000000 ) ;
#12470 = CARTESIAN_POINT ( 'NONE',  ( 5.558508435838283468, 2.857531096718750607, 24.49999999999999289 ) ) ;
#12471 = CARTESIAN_POINT ( 'NONE',  ( -6.369687763352338550E-16, 186.8999999978150584, 9.500000000000001776 ) ) ;
#12472 = CARTESIAN_POINT ( 'NONE',  ( 3.659182332138577465E-16, 202.3202208672780102, 7.308763624242801349 ) ) ;
#12473 = CYLINDRICAL_SURFACE ( 'NONE', #999, 2.499999999999999556 ) ;
#12474 = CARTESIAN_POINT ( 'NONE',  ( 5.866817325727553545, -1.260653813891763120, 25.30022217383879024 ) ) ;
#12475 = CARTESIAN_POINT ( 'NONE',  ( 2.894817532740828536, 189.8405166879407489, 8.135858506145497770 ) ) ;
#12476 = DIRECTION ( 'NONE',  ( -1.000000000000000000, 3.326610055774643275E-18, -1.062480551894329622E-17 ) ) ;
#12477 = CARTESIAN_POINT ( 'NONE',  ( 5.409423237179043831, -2.597448116730963985, 10.88438267301394191 ) ) ;
#12478 = CARTESIAN_POINT ( 'NONE',  ( 2.668367453516690357, -5.373994336898101132, 31.00000000000000000 ) ) ;
#12479 = CARTESIAN_POINT ( 'NONE',  ( 0.09128442572411965550, -0.3999999999999975797, 2.551849451881568420 ) ) ;
#12480 = AXIS2_PLACEMENT_3D ( 'NONE', #7301, #9526, #9772 ) ;
#12481 = CARTESIAN_POINT ( 'NONE',  ( -3.061616997868391523E-16, 189.0000000000000000, -4.500000000000000888 ) ) ;
#12482 = VERTEX_POINT ( 'NONE', #3598 ) ;
#12483 = CARTESIAN_POINT ( 'NONE',  ( -2.066987300000000083, 185.5999999989075775, 6.143825827087054492 ) ) ;
#12484 = VERTEX_POINT ( 'NONE', #13306 ) ;
#12485 = CARTESIAN_POINT ( 'NONE',  ( -5.866923913994597228, -1.260079467906751516, 23.70047945897283270 ) ) ;
#12486 = ORIENTED_EDGE ( 'NONE', *, *, #2586, .F. ) ;
#12487 = PLANE ( 'NONE',  #13668 ) ;
#12488 = CARTESIAN_POINT ( 'NONE',  ( 0.000000000000000000, 22.00000000000000000, 0.000000000000000000 ) ) ;
#12489 = ORIENTED_EDGE ( 'NONE', *, *, #14068, .T. ) ;
#12490 = CIRCLE ( 'NONE', #8189, 1.500000000000001776 ) ;
#12491 = CARTESIAN_POINT ( 'NONE',  ( -1.265664690411614835E-16, 2.066987299999999639, -2.149999998907525800 ) ) ;
#12492 = B_SPLINE_CURVE_WITH_KNOTS ( 'NONE', 3,
 ( #12514, #2971, #421, #346, #9983, #11400, #7822, #5210, #1537, #12590, #1688, #15067, #6565, #11325, #1769, #11244, #4000, #9033 ),
 .UNSPECIFIED., .F., .F.,
 ( 4, 2, 2, 2, 2, 2, 2, 2, 4 ),
 ( 0.003131490185285952174, 0.003522829482338570451, 0.003914168779391188728, 0.004305508076443806571, 0.004696847373496425282, 0.005088186670549043125, 0.005479525967601660968, 0.005870865264654279679, 0.006262204561706897522 ),
 .UNSPECIFIED. ) ;
#12493 = CARTESIAN_POINT ( 'NONE',  ( 1.353717517954364224E-13, 6.000000000000000888, 18.99999999999998934 ) ) ;
#12494 = CARTESIAN_POINT ( 'NONE',  ( -2.843530175656467041, 189.9274080437028829, 6.285367726569456970 ) ) ;
#12495 = CARTESIAN_POINT ( 'NONE',  ( 0.000000000000000000, 184.0000000000000000, -12.49999999999999822 ) ) ;
#12496 = CARTESIAN_POINT ( 'NONE',  ( 2.500000000000000444, 1.035533905932737975, -1.850000000000000533 ) ) ;
#12497 = EDGE_CURVE ( 'NONE', #1820, #15059, #2405, .T. ) ;
#12498 = CARTESIAN_POINT ( 'NONE',  ( -3.922672396097048875, -4.541739265057705310, 10.62635295315574702 ) ) ;
#12499 = CARTESIAN_POINT ( 'NONE',  ( -6.081464507797580410, -1.446657058464413170, 25.37380055247394495 ) ) ;
#12500 = CARTESIAN_POINT ( 'NONE',  ( -1.461580736456472351, -1.461580736456473018, -0.04999999890752505893 ) ) ;
#12501 = CARTESIAN_POINT ( 'NONE',  ( -5.984595133899190955, 1.806709459528622386, 30.00004921015706572 ) ) ;
#12502 = CARTESIAN_POINT ( 'NONE',  ( -0.8002720181890644602, 6.199262377003409874, 30.38606262465555474 ) ) ;
#12503 = ORIENTED_EDGE ( 'NONE', *, *, #4450, .F. ) ;
#12504 = AXIS2_PLACEMENT_3D ( 'NONE', #8586, #12297, #2524 ) ;
#12505 = ORIENTED_EDGE ( 'NONE', *, *, #15149, .T. ) ;
#12506 = EDGE_LOOP ( 'NONE', ( #4356, #13385 ) ) ;
#12507 = CARTESIAN_POINT ( 'NONE',  ( 5.783198643800777639, -1.602922020054677432, 30.02622176056706493 ) ) ;
#12508 = CARTESIAN_POINT ( 'NONE',  ( -0.05280746222630467585, 189.0001365486126303, 9.499442212161147481 ) ) ;
#12509 = ORIENTED_EDGE ( 'NONE', *, *, #11938, .T. ) ;
#12510 = CARTESIAN_POINT ( 'NONE',  ( -5.903061651806559063, -2.057626436184912144, 17.00008258189709309 ) ) ;
#12511 = CARTESIAN_POINT ( 'NONE',  ( -3.634089073485469168, -4.776071126502662523, 18.99992002356260912 ) ) ;
#12512 = EDGE_CURVE ( 'NONE', #4630, #5531, #9671, .T. ) ;
#12513 = CARTESIAN_POINT ( 'NONE',  ( -0.6139731865238436948, 6.220476368274066914, 17.19975545601930733 ) ) ;
#12514 = CARTESIAN_POINT ( 'NONE',  ( 1.354942165116848791E-13, 6.250000000000000888, 16.99999999999998579 ) ) ;
#12515 = CARTESIAN_POINT ( 'NONE',  ( 2.500000000000000444, 186.2499999978150527, 8.035533905932739529 ) ) ;
#12516 = CIRCLE ( 'NONE', #8472, 3.000000000000000888 ) ;
#12517 = CARTESIAN_POINT ( 'NONE',  ( -3.567258970016013553, 5.133675764669650476, 10.49991780678442232 ) ) ;
#12518 = CARTESIAN_POINT ( 'NONE',  ( 4.286401442266483564, 4.198423832313243231, 11.49999999999998224 ) ) ;
#12519 = DIRECTION ( 'NONE',  ( 0.000000000000000000, 1.000000000000000000, 0.000000000000000000 ) ) ;
#12520 = CARTESIAN_POINT ( 'NONE',  ( 2.500000000000000444, 185.5199999975965852, 8.035533905932739529 ) ) ;
#12521 = CARTESIAN_POINT ( 'NONE',  ( -1.939606487604890850, 228.4085856529902117, 7.419409526801750587 ) ) ;
#12522 = EDGE_CURVE ( 'NONE', #28, #14650, #11216, .T. ) ;
#12523 = CARTESIAN_POINT ( 'NONE',  ( -2.734462099041327310, 226.8914831935726966, 6.155496219900511434 ) ) ;
#12524 = CARTESIAN_POINT ( 'NONE',  ( -1.967390401563962055, 189.1241570952389850, 9.449926551978856892 ) ) ;
#12525 = EDGE_CURVE ( 'NONE', #15709, #9577, #2398, .T. ) ;
#12526 = ORIENTED_EDGE ( 'NONE', *, *, #15436, .F. ) ;
#12527 = CARTESIAN_POINT ( 'NONE',  ( -4.286401442266592809, 4.198423832313131321, 5.000000000000004441 ) ) ;
#12528 = CARTESIAN_POINT ( 'NONE',  ( -5.648559266344472363, 2.676764518776052704, 23.88603820591928084 ) ) ;
#12529 = CARTESIAN_POINT ( 'NONE',  ( -4.267838854167295359, 4.217593933790213079, 24.23760108194401397 ) ) ;
#12530 = CARTESIAN_POINT ( 'NONE',  ( 5.859155363331391086, 2.178872204144949531, 12.47400098023328852 ) ) ;
#12531 = CARTESIAN_POINT ( 'NONE',  ( 9.750000000000003553, 184.0000000000000000, -1.499999999999897415 ) ) ;
#12532 = CARTESIAN_POINT ( 'NONE',  ( 3.312524433819711511, -5.004191858254047887, 23.52591947216898660 ) ) ;
#12533 = CARTESIAN_POINT ( 'NONE',  ( -0.8561741729129458411, -2.066987299999999195, -2.399999998907525356 ) ) ;
#12534 = CARTESIAN_POINT ( 'NONE',  ( 9.750000000000003553, 182.0000000000000000, 1.500000000000101696 ) ) ;
#12535 =( LENGTH_UNIT ( ) NAMED_UNIT ( * ) SI_UNIT ( .MILLI., .METRE. ) );
#12536 = ADVANCED_FACE ( 'NONE', ( #5580 ), #9467, .F. ) ;
#12537 = COLOUR_RGB ( '', 0.40784314, 0.44705882, 0.49803922) ;
#12538 = DIRECTION ( 'NONE',  ( 0.5877852522924802425, -0.8090169943749422332, 0.000000000000000000 ) ) ;
#12539 = CARTESIAN_POINT ( 'NONE',  ( -2.500000000000000444, 185.9500000000000455, 5.964466094067261359 ) ) ;
#12540 = CARTESIAN_POINT ( 'NONE',  ( -3.061616997868386099E-16, 189.0000000000000000, 7.000000000000000000 ) ) ;
#12541 = CARTESIAN_POINT ( 'NONE',  ( 0.4540882845019501568, 227.6260587419843091, 5.159427175404782240 ) ) ;
#12542 = CARTESIAN_POINT ( 'NONE',  ( -2.066987299999999195, -0.8561741729129467293, -1.699999998907525400 ) ) ;
#12543 = CARTESIAN_POINT ( 'NONE',  ( 6.176542424588150837, -0.9554180641283406272, 24.63063932754212004 ) ) ;
#12544 = CARTESIAN_POINT ( 'NONE',  ( -6.000000000000000888, 0.000000000000000000, 36.00000000000000711 ) ) ;
#12545 = EDGE_CURVE ( 'NONE', #5531, #5264, #11609, .T. ) ;
#12546 = CARTESIAN_POINT ( 'NONE',  ( -0.8561741729129471734, 187.9999999989075263, 9.066987300000000971 ) ) ;
#12547 = DIRECTION ( 'NONE',  ( -0.5877852522924685852, -0.8090169943749507819, 0.000000000000000000 ) ) ;
#12549 = ORIENTED_EDGE ( 'NONE', *, *, #5329, .T. ) ;
#12548 = CARTESIAN_POINT ( 'NONE',  ( 2.066987299999999639, 189.2499999989075263, 7.000000000000000000 ) ) ;
#12550 = FACE_BOUND ( 'NONE', #6468, .T. ) ;
#12551 = CARTESIAN_POINT ( 'NONE',  ( 5.858736126997183824, -2.179962889276933602, 12.47359571723299965 ) ) ;
#12552 = CARTESIAN_POINT ( 'NONE',  ( -5.999999999999999112, 202.3202208672780102, 7.308763624254441815 ) ) ;
#12553 = ADVANCED_FACE ( 'NONE', ( #14298 ), #9476, .T. ) ;
#12554 = CARTESIAN_POINT ( 'NONE',  ( 2.939309742956421889, 189.2553574017071867, 7.797426251816824916 ) ) ;
#12555 = DIRECTION ( 'NONE',  ( -0.000000000000000000, 1.000000000000000000, -0.000000000000000000 ) ) ;
#12556 = CARTESIAN_POINT ( 'NONE',  ( 4.286401442266591033, -4.198423832313133097, 5.132360785839115813 ) ) ;
#12557 = CARTESIAN_POINT ( 'NONE',  ( 6.021135683317753617, -1.680226122398018163, 23.52622717124730656 ) ) ;
#12558 = EDGE_CURVE ( 'NONE', #4806, #10183, #14294, .T. ) ;
#12559 = CARTESIAN_POINT ( 'NONE',  ( 0.5662760513513177552, -0.3999999999999975797, 2.593905796087984328 ) ) ;
#12560 = CARTESIAN_POINT ( 'NONE',  ( -1.262974410557502258, 189.0000000000000000, 4.817524377743032993 ) ) ;
#12561 = EDGE_LOOP ( 'NONE', ( #12549, #1815, #7798, #4216 ) ) ;
#12562 = CARTESIAN_POINT ( 'NONE',  ( 0.8561741729129452860, 187.7999999989075093, 4.933012699999999029 ) ) ;
#12563 = VERTEX_POINT ( 'NONE', #10729 ) ;
#12564 = CARTESIAN_POINT ( 'NONE',  ( -5.782947755040608762, -1.603807858344187487, 23.52601979877760030 ) ) ;
#12565 = CIRCLE ( 'NONE', #3927, 2.000000000000000000 ) ;
#12566 = ORIENTED_EDGE ( 'NONE', *, *, #11920, .F. ) ;
#12567 = DIRECTION ( 'NONE',  ( 0.000000000000000000, 0.000000000000000000, 1.000000000000000000 ) ) ;
#12568 = CARTESIAN_POINT ( 'NONE',  ( -4.322356511625935482, 7.650514973136391284, 24.49999999999999289 ) ) ;
#12569 = ORIENTED_EDGE ( 'NONE', *, *, #943, .T. ) ;
#12570 = CARTESIAN_POINT ( 'NONE',  ( 2.066987299999999639, 2.531329380823229670E-16, 0.8500000010924746441 ) ) ;
#12571 = CARTESIAN_POINT ( 'NONE',  ( -3.159082487394791361, 5.393634094348326080, 4.200455375311574535 ) ) ;
#12572 = CARTESIAN_POINT ( 'NONE',  ( 2.066987299999999639, 189.2999999989075377, 6.143825827087054492 ) ) ;
#12573 = CARTESIAN_POINT ( 'NONE',  ( -2.500000000000000000, 0.000000000000000000, -1.500000000000000000 ) ) ;
#12574 = DIRECTION ( 'NONE',  ( 0.000000000000000000, 0.000000000000000000, -1.000000000000000000 ) ) ;
#12575 = AXIS2_PLACEMENT_3D ( 'NONE', #14903, #2572, #3991 ) ;
#12576 = CARTESIAN_POINT ( 'NONE',  ( 6.123233995736766282E-16, -6.250000000000000888, 5.000000000000004441 ) ) ;
#12577 = CONTEXT_DEPENDENT_SHAPE_REPRESENTATION ( #14637, #5779 ) ;
#12578 = CARTESIAN_POINT ( 'NONE',  ( -5.317509234263873452, 2.779225709351156315, 24.49999999999999289 ) ) ;
#12579 = CARTESIAN_POINT ( 'NONE',  ( -1.265664690411614835E-16, 2.066987299999999639, 1.250000001092474777 ) ) ;
#12580 = CARTESIAN_POINT ( 'NONE',  ( -2.500000000000000444, 186.6999999978150697, 7.000000000000000000 ) ) ;
#12581 = VERTEX_POINT ( 'NONE', #14466 ) ;
#12582 = ORIENTED_EDGE ( 'NONE', *, *, #13392, .T. ) ;
#12583 = ORIENTED_EDGE ( 'NONE', *, *, #9643, .F. ) ;
#12584 = CARTESIAN_POINT ( 'NONE',  ( -5.558508435838158235, -2.857531096718993080, 11.36939309276498911 ) ) ;
#12585 = CARTESIAN_POINT ( 'NONE',  ( 0.000000000000000000, 22.00000000000000000, -7.000000000000000000 ) ) ;
#12586 = ORIENTED_EDGE ( 'NONE', *, *, #1912, .T. ) ;
#12587 = CARTESIAN_POINT ( 'NONE',  ( -25.39999999999994884, 0.000000000000000000, 0.000000000000000000 ) ) ;
#12588 = CARTESIAN_POINT ( 'NONE',  ( -2.668367453516752974, -5.373994336898072710, 17.99999999999998934 ) ) ;
#12589 = CARTESIAN_POINT ( 'NONE',  ( -0.1323736289504275354, 6.250000000000000000, 18.99999999999997158 ) ) ;
#12590 = CARTESIAN_POINT ( 'NONE',  ( 1.000082492230843334, 6.169467968613687070, 18.13152538105398293 ) ) ;
#12591 = CARTESIAN_POINT ( 'NONE',  ( -2.500000000000000444, 187.4999999978150527, 7.000000000000000000 ) ) ;
#12592 = CARTESIAN_POINT ( 'NONE',  ( -1.767766952966368432, -1.767766952966369320, 1.806999999978150528 ) ) ;
#12593 = CARTESIAN_POINT ( 'NONE',  ( 3.735808404764946467, 4.696639218303165997, 10.52601979877758787 ) ) ;
#12594 = CARTESIAN_POINT ( 'NONE',  ( -1.035533905932739529, 185.3199999975965682, 9.500000000000003553 ) ) ;
#12595 = CARTESIAN_POINT ( 'NONE',  ( 1.237590631448066469, 228.1696616696178808, 9.916980740552745033 ) ) ;
#12596 = CIRCLE ( 'NONE', #6013, 2.000000000000000000 ) ;
#12597 = CARTESIAN_POINT ( 'NONE',  ( -2.999982576790682476, 227.2579145021288696, 7.234552515775640735 ) ) ;
#12598 = ORIENTED_EDGE ( 'NONE', *, *, #3765, .T. ) ;
#12599 = EDGE_CURVE ( 'NONE', #2728, #5689, #5546, .T. ) ;
#12600 = CARTESIAN_POINT ( 'NONE',  ( -1.785019455104270181, -1.755996401752895286, -2.500026767917371107 ) ) ;
#12601 = VERTEX_POINT ( 'NONE', #15510 ) ;
#12602 = EDGE_CURVE ( 'NONE', #3171, #15527, #14420, .T. ) ;
#12603 = CARTESIAN_POINT ( 'NONE',  ( -2.668367453516708565, 5.373994336898094026, 5.000000000000004441 ) ) ;
#12604 = CARTESIAN_POINT ( 'NONE',  ( -6.176542424588088664, 0.9554180641287480791, 24.49999999999999289 ) ) ;
#12605 = CARTESIAN_POINT ( 'NONE',  ( -0.6139731865239884678, 6.220476368274053591, 4.199755456019329536 ) ) ;
#12606 = CARTESIAN_POINT ( 'NONE',  ( 5.558508435838199979, 2.857531096718914476, 31.00000000000000000 ) ) ;
#12607 = CARTESIAN_POINT ( 'NONE',  ( 0.3830661952130403614, 228.2493291729371094, 10.15124818647456451 ) ) ;
#12608 = AXIS2_PLACEMENT_3D ( 'NONE', #1347, #3735, #8612 ) ;
#12609 = EDGE_CURVE ( 'NONE', #1532, #14984, #12893, .T. ) ;
#12610 = CARTESIAN_POINT ( 'NONE',  ( -3.781065399485938894, -4.978303713186498669, 31.99991741810289625 ) ) ;
#12611 = CARTESIAN_POINT ( 'NONE',  ( -2.500000000000000000, -1.035533905932739307, 1.750000000000000222 ) ) ;
#12612 = CARTESIAN_POINT ( 'NONE',  ( -4.286401442266546624, -4.198423832313178394, 31.00000000000000000 ) ) ;
#12613 = SURFACE_STYLE_FILL_AREA ( #4022 ) ;
#12614 = CARTESIAN_POINT ( 'NONE',  ( -3.255128505894239854, -5.336774832660761803, 30.12619944752604084 ) ) ;
#12615 = CARTESIAN_POINT ( 'NONE',  ( -2.500000000000000444, 186.7999999999999829, 7.000000000000000000 ) ) ;
#12616 = CARTESIAN_POINT ( 'NONE',  ( -0.5154556838971166011, 227.6308307018634025, 5.173208867712369319 ) ) ;
#12617 = UNCERTAINTY_MEASURE_WITH_UNIT (LENGTH_MEASURE( 1.000000000000000082E-05 ), #9056, 'distance_accuracy_value', 'NONE');
#12618 = DIRECTION ( 'NONE',  ( -1.000000000000000000, 0.000000000000000000, 0.000000000000000000 ) ) ;
#12619 = CARTESIAN_POINT ( 'NONE',  ( 3.459597053047784865, 5.206576120509786243, 12.47408542334169113 ) ) ;
#12620 = AXIS2_PLACEMENT_3D ( 'NONE', #6199, #11036, #9789 ) ;
#12621 = CARTESIAN_POINT ( 'NONE',  ( 2.066987299999999639, 0.8561741729129456191, 1.700000001092474733 ) ) ;
#12622 = CARTESIAN_POINT ( 'NONE',  ( -1.035533905932737753, 185.0499999999999829, 4.500000000000000888 ) ) ;
#12623 = CARTESIAN_POINT ( 'NONE',  ( -3.922672396097174552, 4.541739265057599617, 18.87364704684421923 ) ) ;
#12625 = ORIENTED_EDGE ( 'NONE', *, *, #5440, .F. ) ;
#12624 = CARTESIAN_POINT ( 'NONE',  ( -2.066987300000000527, 188.0499999989075093, 7.000000000000000000 ) ) ;
#12626 = CARTESIAN_POINT ( 'NONE',  ( -4.005361199355057522, -4.468319061418718263, 17.19977782616121686 ) ) ;
#12627 = CARTESIAN_POINT ( 'NONE',  ( 2.500000000000000444, 187.0499999978150356, 8.035533905932739529 ) ) ;
#12628 = AXIS2_PLACEMENT_3D ( 'NONE', #380, #5330, #3956 ) ;
#12629 = CARTESIAN_POINT ( 'NONE',  ( 3.659182332138577465E-16, 215.0542865858234336, 7.296348638359030581 ) ) ;
#12630 = CARTESIAN_POINT ( 'NONE',  ( 2.493490693894865551, 188.9999999989163655, 6.752556059726261495 ) ) ;
#12631 = CARTESIAN_POINT ( 'NONE',  ( 0.0005321174777195292194, -0.3999999999999906408, -2.461401996259243496 ) ) ;
#12632 = CARTESIAN_POINT ( 'NONE',  ( -0.9999502950801862911, 5.916088184763887092, 31.13108149190011176 ) ) ;
#12633 = CARTESIAN_POINT ( 'NONE',  ( 2.451648050241212129, 189.9784261975811717, 5.460752168824765107 ) ) ;
#12634 = DIRECTION ( 'NONE',  ( -0.9510565162951545304, 0.3090169943749447867, 0.000000000000000000 ) ) ;
#12635 = CARTESIAN_POINT ( 'NONE',  ( -9.750000000000003553, 182.0000000000000000, -1.500000000000033751 ) ) ;
#12636 = EDGE_CURVE ( 'NONE', #6786, #6402, #13740, .T. ) ;
#12637 = CARTESIAN_POINT ( 'NONE',  ( -5.375605342016462451, -2.665598297262376182, 10.99687951097621408 ) ) ;
#12638 = ORIENTED_EDGE ( 'NONE', *, *, #13872, .T. ) ;
#12639 = CARTESIAN_POINT ( 'NONE',  ( -0.8561741729129469514, 188.1999999989075150, 9.066987299999999195 ) ) ;
#12640 = DIRECTION ( 'NONE',  ( 0.000000000000000000, 0.3271946967975951637, 0.9449569463142382109 ) ) ;
#12641 = EDGE_LOOP ( 'NONE', ( #13907, #14844, #569, #7145 ) ) ;
#12642 = FACE_OUTER_BOUND ( 'NONE', #2552, .T. ) ;
#12643 = EDGE_LOOP ( 'NONE', ( #4309, #13849 ) ) ;
#12644 = ADVANCED_FACE ( 'NONE', ( #10088 ), #297, .F. ) ;
#12645 = CARTESIAN_POINT ( 'NONE',  ( 0.000000000000000000, 184.0000000000000000, 0.000000000000000000 ) ) ;
#12646 = CARTESIAN_POINT ( 'NONE',  ( -1.035533905932737975, 185.8500000000000227, 4.500000000000001776 ) ) ;
#12647 = EDGE_LOOP ( 'NONE', ( #13143, #13310, #3682, #6709 ) ) ;
#12648 = CARTESIAN_POINT ( 'NONE',  ( -5.665308849928812229, -1.980336949702540261, 30.00007997643738022 ) ) ;
#12649 = ADVANCED_FACE ( 'NONE', ( #11198 ), #5242, .F. ) ;
#12650 = CARTESIAN_POINT ( 'NONE',  ( 0.5042987395407738660, 5.979983180450076041, 5.873293041799771963 ) ) ;
#12651 = VECTOR ( 'NONE', #1404, 1000.000000000000000 ) ;
#12652 = CARTESIAN_POINT ( 'NONE',  ( 5.783198643800823824, -1.602922020054500463, 23.52622176056705783 ) ) ;
#12653 = CARTESIAN_POINT ( 'NONE',  ( 2.500000000000000444, 1.035533905932737975, -0.2500000000000002220 ) ) ;
#12654 = CARTESIAN_POINT ( 'NONE',  ( -5.615973259022306152, -2.743340227996199587, 5.503892131249681796 ) ) ;
#12655 = AXIS2_PLACEMENT_3D ( 'NONE', #13980, #3390, #10560 ) ;
#12656 = DIRECTION ( 'NONE',  ( -0.000000000000000000, -1.000000000000000000, -0.000000000000000000 ) ) ;
#12657 = CARTESIAN_POINT ( 'NONE',  ( -1.530808498934191571E-16, 2.500000000000000000, -2.562499999726881139 ) ) ;
#12658 = CARTESIAN_POINT ( 'NONE',  ( -7.490007020835705909, -2.433650805992367161, 5.000000000000004441 ) ) ;
#12659 = CARTESIAN_POINT ( 'NONE',  ( -2.066987299999999195, -0.8561741729129466183, -0.8999999989075251339 ) ) ;
#12660 = CARTESIAN_POINT ( 'NONE',  ( 2.094888806938587637E-14, 6.250000000000000888, 30.00000000000000000 ) ) ;
#12661 = EDGE_LOOP ( 'NONE', ( #10845, #13833 ) ) ;
#12662 = VERTEX_POINT ( 'NONE', #12544 ) ;
#12663 = AXIS2_PLACEMENT_3D ( 'NONE', #1388, #6263, #7600 ) ;
#12664 = ORIENTED_EDGE ( 'NONE', *, *, #8143, .T. ) ;
#12665 = CARTESIAN_POINT ( 'NONE',  ( 3.458623254138732950, -5.207221900902805345, 12.47377282875266324 ) ) ;
#12666 = CARTESIAN_POINT ( 'NONE',  ( 5.858736126997123428, 2.179962889277093918, 4.026404282766995912 ) ) ;
#12667 = ORIENTED_EDGE ( 'NONE', *, *, #14471, .T. ) ;
#12668 = CARTESIAN_POINT ( 'NONE',  ( 5.843075991566613503, -1.368655265450920533, 18.87364704684421923 ) ) ;
#12669 = CARTESIAN_POINT ( 'NONE',  ( -2.500000000000000444, 1.035533905932737753, 0.9500000021849496212 ) ) ;
#12670 = CARTESIAN_POINT ( 'NONE',  ( -3.567624405365311446, 5.133384272590732600, 31.99995078984293428 ) ) ;
#12671 = CARTESIAN_POINT ( 'NONE',  ( 5.726049995854478603, -2.506679546901855460, 30.20045537531156654 ) ) ;
#12672 = CARTESIAN_POINT ( 'NONE',  ( 1.767766952966369098, 187.1999999978150697, 5.232233047033630235 ) ) ;
#12673 = DIRECTION ( 'NONE',  ( 0.5877852522924802425, -0.8090169943749422332, 0.000000000000000000 ) ) ;
#12674 = APPLICATION_CONTEXT ( 'automotive_design' ) ;
#12675 = CARTESIAN_POINT ( 'NONE',  ( 0.09999999999998898659, 0.000000000000000000, 0.000000000000000000 ) ) ;
#12676 = VECTOR ( 'NONE', #5867, 1000.000000000000000 ) ;
#12677 = CARTESIAN_POINT ( 'NONE',  ( 1.035533905932737753, 189.7199999975965738, 4.500000000000000888 ) ) ;
#12678 = CARTESIAN_POINT ( 'NONE',  ( 0.1954887924997270876, 228.2535971796124556, 10.16375797564445804 ) ) ;
#12679 = CARTESIAN_POINT ( 'NONE',  ( -1.865818183961493126, 226.5341093703536899, 5.102530190813160615 ) ) ;
#12680 = B_SPLINE_CURVE_WITH_KNOTS ( 'NONE', 3,
 ( #15145, #14991, #502, #4082, #7743, #1687, #5369, #15066, #4162, #9032, #5445, #2970, #10291, #4239, #10367, #9108, #7900, #12741 ),
 .UNSPECIFIED., .F., .F.,
 ( 4, 2, 2, 2, 2, 2, 2, 2, 4 ),
 ( 0.003131918686235971288, 0.003523310662250261124, 0.003914702638264550526, 0.004306094614278840361, 0.004697486590293130197, 0.005088878566307420033, 0.005480270542321709869, 0.005871662518335999704, 0.006263054494350289540 ),
 .UNSPECIFIED. ) ;
#12681 = EDGE_LOOP ( 'NONE', ( #800, #5841 ) ) ;
#12682 = CARTESIAN_POINT ( 'NONE',  ( 3.922288969639853295, -4.542045818322462125, 4.126215691297385746 ) ) ;
#12683 = ORIENTED_EDGE ( 'NONE', *, *, #10429, .T. ) ;
#12684 = DIRECTION ( 'NONE',  ( 0.5877852522924802425, -0.8090169943749422332, 0.000000000000000000 ) ) ;
#12685 = CARTESIAN_POINT ( 'NONE',  ( 1.035533905932737753, 189.6499999978150584, 4.500000000000001776 ) ) ;
#12686 = CARTESIAN_POINT ( 'NONE',  ( 0.2619041840695610635, -6.245686665308499919, 10.52605849433793495 ) ) ;
#12687 = CARTESIAN_POINT ( 'NONE',  ( -0.9735856429312839122, 5.920699391845025694, 5.262852839067274857 ) ) ;
#12688 = CARTESIAN_POINT ( 'NONE',  ( 2.587737285089668493, 227.7819843651293183, 8.776849827616773680 ) ) ;
#12689 = CARTESIAN_POINT ( 'NONE',  ( 4.416779112813651764, 4.422345839825798208, 5.262252817217140333 ) ) ;
#12690 = CARTESIAN_POINT ( 'NONE',  ( 2.817313151351064970, -5.579000502529494199, 17.86936067245787285 ) ) ;
#12691 = CARTESIAN_POINT ( 'NONE',  ( 1.767766952966368654, 1.767766952966369098, -0.2000000000000000944 ) ) ;
#12692 = CARTESIAN_POINT ( 'NONE',  ( 3.311576095066571579, 5.004818610361311926, 4.026221760567070262 ) ) ;
#12693 = CARTESIAN_POINT ( 'NONE',  ( -4.070051655338055241, -4.744673454622520659, 30.12632671364007564 ) ) ;
#12694 = CARTESIAN_POINT ( 'NONE',  ( 1.035533905932738419, 185.4499999999999886, 9.500000000000003553 ) ) ;
#12695 = EDGE_CURVE ( 'NONE', #1447, #12563, #450, .T. ) ;
#12696 = CARTESIAN_POINT ( 'NONE',  ( 1.498060502294345175, 227.8308734224802095, 5.750943654540091821 ) ) ;
#12697 = DIRECTION ( 'NONE',  ( 0.000000000000000000, 0.000000000000000000, 1.000000000000000000 ) ) ;
#12698 = CARTESIAN_POINT ( 'NONE',  ( 6.143143148203090043, -1.154591847827534101, 25.11396179408070850 ) ) ;
#12699 = CARTESIAN_POINT ( 'NONE',  ( -0.8561741729129455081, 2.066987299999999639, -0.4999999989075253892 ) ) ;
#12700 = EDGE_CURVE ( 'NONE', #8455, #1570, #7431, .T. ) ;
#12701 = CARTESIAN_POINT ( 'NONE',  ( -2.500000000000000888, 188.3999999999999773, 7.000000000000000000 ) ) ;
#12702 = DIRECTION ( 'NONE',  ( 0.000000000000000000, 0.000000000000000000, 1.000000000000000000 ) ) ;
#12704 = EDGE_LOOP ( 'NONE', ( #11465, #15134 ) ) ;
#12703 = CARTESIAN_POINT ( 'NONE',  ( -2.066987300000000527, 186.4999999989074695, 7.856174172912944620 ) ) ;
#12705 = FACE_BOUND ( 'NONE', #3361, .T. ) ;
#12706 = CARTESIAN_POINT ( 'NONE',  ( -4.286401442266688733, 4.198423832313033621, 17.99999999999998934 ) ) ;
#12707 = CARTESIAN_POINT ( 'NONE',  ( 0.5662760513513177552, 0.4000000000000062395, -2.593905796088003424 ) ) ;
#12708 = EDGE_CURVE ( 'NONE', #8865, #9005, #1547, .T. ) ;
#12709 = CARTESIAN_POINT ( 'NONE',  ( 1.482061430985168737, 189.7295665886300924, 9.997153617204970644 ) ) ;
#12710 = CARTESIAN_POINT ( 'NONE',  ( 0.000000000000000000, -0.3999999999999958589, -2.450963827680254337 ) ) ;
#12711 = CARTESIAN_POINT ( 'NONE',  ( -0.9740807849835945165, 5.920620690450692614, 30.73850119700669126 ) ) ;
#12712 = CARTESIAN_POINT ( 'NONE',  ( 1.724621985266778568, 228.5864789591000488, 7.933175541215780946 ) ) ;
#12713 = CARTESIAN_POINT ( 'NONE',  ( -4.286401442266607908, 4.198423832313116222, 30.86938304467861016 ) ) ;
#12714 = CARTESIAN_POINT ( 'NONE',  ( 0.000000000000000000, 0.000000000000000000, 0.000000000000000000 ) ) ;
#12715 = FACE_OUTER_BOUND ( 'NONE', #14446, .T. ) ;
#12716 = ORIENTED_EDGE ( 'NONE', *, *, #7862, .F. ) ;
#12717 = CARTESIAN_POINT ( 'NONE',  ( -0.8561741729129470624, 186.3999999989075320, 9.066987300000000971 ) ) ;
#12718 = ORIENTED_EDGE ( 'NONE', *, *, #11282, .T. ) ;
#12719 = DIRECTION ( 'NONE',  ( 0.000000000000000000, 0.000000000000000000, -1.000000000000000000 ) ) ;
#12720 = VERTEX_POINT ( 'NONE', #4667 ) ;
#12721 = CARTESIAN_POINT ( 'NONE',  ( 2.094888799673178700E-14, -6.250000000000000888, 30.00000000000000000 ) ) ;
#12722 = CARTESIAN_POINT ( 'NONE',  ( -2.668367453516630849, -5.373994336898132218, 5.000000000000004441 ) ) ;
#12723 = CARTESIAN_POINT ( 'NONE',  ( -2.841519077896158318, 5.566940434250007286, 4.736203831591942581 ) ) ;
#12724 = CARTESIAN_POINT ( 'NONE',  ( 5.843318061569099164, -1.367618216965411637, 23.62696220972947359 ) ) ;
#12725 = VECTOR ( 'NONE', #10309, 1000.000000000000000 ) ;
#12726 = CARTESIAN_POINT ( 'NONE',  ( 2.500000000000000000, 3.061616997868383141E-16, 1.400000002184949910 ) ) ;
#12727 = CARTESIAN_POINT ( 'NONE',  ( -5.558508435838188433, -2.857531096718933128, 5.130639327542137806 ) ) ;
#12728 = CARTESIAN_POINT ( 'NONE',  ( -4.267992336621177607, -4.217442018460021202, 11.23805675996852216 ) ) ;
#12729 = CARTESIAN_POINT ( 'NONE',  ( 0.8561741729129451750, 2.066987299999999639, -1.999999998907525223 ) ) ;
#12730 = ADVANCED_FACE ( 'NONE', ( #3698 ), #3382, .F. ) ;
#12731 = CARTESIAN_POINT ( 'NONE',  ( 0.000000000000000000, 0.000000000000000000, 2.500000000000000000 ) ) ;
#12732 = EDGE_CURVE ( 'NONE', #8051, #9247, #5533, .T. ) ;
#12733 = ORIENTED_EDGE ( 'NONE', *, *, #15177, .T. ) ;
#12734 = ORIENTED_EDGE ( 'NONE', *, *, #9801, .F. ) ;
#12735 = ORIENTED_EDGE ( 'NONE', *, *, #6115, .F. ) ;
#12736 = CARTESIAN_POINT ( 'NONE',  ( 3.158296126777861978, -5.394094919772070007, 12.29887838423337953 ) ) ;
#12737 = CARTESIAN_POINT ( 'NONE',  ( 0.000000000000000000, 0.000000000000000000, 2.500000000000000000 ) ) ;
#12738 = EDGE_LOOP ( 'NONE', ( #4467, #8054, #13762, #981 ) ) ;
#12739 = CARTESIAN_POINT ( 'NONE',  ( 2.897581130414634077E-17, 22.00000000000000000, 9.750000000000003553 ) ) ;
#12740 = CARTESIAN_POINT ( 'NONE',  ( -2.500000000000000000, -1.035533905932739307, 1.050000002184949599 ) ) ;
#12741 = CARTESIAN_POINT ( 'NONE',  ( -5.935543223013861613, 0.8771126767606655106, 5.000000000000004441 ) ) ;
#12742 = CARTESIAN_POINT ( 'NONE',  ( 0.7081379353438689295, -0.3999999999999906408, -2.606463079733445376 ) ) ;
#12743 = CARTESIAN_POINT ( 'NONE',  ( 1.035533905932738197, 189.3499999978150754, 9.500000000000003553 ) ) ;
#12744 = DIRECTION ( 'NONE',  ( 0.000000000000000000, -1.570965579844596505E-14, -1.000000000000000000 ) ) ;
#12745 = CARTESIAN_POINT ( 'NONE',  ( 5.531757352715618303, 2.326874507723293295, 18.87380682714709579 ) ) ;
#12746 = CIRCLE ( 'NONE', #5398, 2.500000000000000000 ) ;
#12747 = CARTESIAN_POINT ( 'NONE',  ( -5.486741141153776091, -2.429871531109769389, 4.201117577520603774 ) ) ;
#12748 = CARTESIAN_POINT ( 'NONE',  ( -0.5160604560792059203, 228.8899596144369752, 8.809644983231040172 ) ) ;
#12749 = LINE ( 'NONE', #975, #7254 ) ;
#12750 = EDGE_CURVE ( 'NONE', #1061, #9576, #2110, .T. ) ;
#12751 = VERTEX_POINT ( 'NONE', #1153 ) ;
#12752 = CARTESIAN_POINT ( 'NONE',  ( 0.9998469633096263021, -2.309553665790732957, -2.499997523255642840 ) ) ;
#12753 = ORIENTED_EDGE ( 'NONE', *, *, #9912, .T. ) ;
#12754 = CARTESIAN_POINT ( 'NONE',  ( 4.290130679986631890, -4.545972905167674050, 5.615601928929212505 ) ) ;
#12755 = CARTESIAN_POINT ( 'NONE',  ( 5.940390500375388072, 6.474944468551740329, 24.49999999999999289 ) ) ;
#12756 = CARTESIAN_POINT ( 'NONE',  ( 9.825582188149883933E-17, 184.4499999989075150, 4.933012699999999029 ) ) ;
#12757 = CARTESIAN_POINT ( 'NONE',  ( 1.734723475976807094E-15, 0.000000000000000000, 13.50000000000000000 ) ) ;
#12758 = CARTESIAN_POINT ( 'NONE',  ( -5.487348639458843103, 2.428538342494515501, 17.19977782616120976 ) ) ;
#12759 = FACE_BOUND ( 'NONE', #7639, .T. ) ;
#12760 = CARTESIAN_POINT ( 'NONE',  ( 2.500000000000000444, -1.035533905932737309, 0.4499999999999998446 ) ) ;
#12761 = DIRECTION ( 'NONE',  ( -1.000000000000000000, 0.000000000000000000, 0.000000000000000000 ) ) ;
#12762 = APPLICATION_PROTOCOL_DEFINITION ( 'draft international standard', 'automotive_design', 1998, #7797 ) ;
#12763 = CARTESIAN_POINT ( 'NONE',  ( 5.330189595673604508, 2.755293208590308573, 5.263826032055957782 ) ) ;
#12764 = CARTESIAN_POINT ( 'NONE',  ( -2.500000000000000444, 185.8499999978150754, 5.964466094067261359 ) ) ;
#12765 = ADVANCED_FACE ( 'NONE', ( #9600 ), #15471, .T. ) ;
#12766 = CARTESIAN_POINT ( 'NONE',  ( -1.159640499634989608, 227.7308148186401979, 5.461968699681960082 ) ) ;
#12767 = FACE_BOUND ( 'NONE', #13352, .T. ) ;
#12768 = AXIS2_PLACEMENT_3D ( 'NONE', #5777, #3220, #2342 ) ;
#12769 = CARTESIAN_POINT ( 'NONE',  ( -5.935543223013841185, 0.8771126767608004027, 17.99999999999998934 ) ) ;
#12770 = CARTESIAN_POINT ( 'NONE',  ( -2.066987299999999639, 0.8561741729129455081, -1.999999998907525001 ) ) ;
#12771 = CARTESIAN_POINT ( 'NONE',  ( 1.035533905932738197, 187.0499999999999829, 9.500000000000003553 ) ) ;
#12772 = CARTESIAN_POINT ( 'NONE',  ( 2.817313151351004130, -5.579000502529524397, 24.49999999999999289 ) ) ;
#12774 = EDGE_LOOP ( 'NONE', ( #14484, #9086, #6537, #11356 ) ) ;
#12773 = DIRECTION ( 'NONE',  ( 1.000000000000000000, 0.000000000000000000, 0.000000000000000000 ) ) ;
#12775 = CARTESIAN_POINT ( 'NONE',  ( 0.7081379353438682633, 0.4000000000000061839, 2.606463079733442711 ) ) ;
#12776 = B_SPLINE_CURVE_WITH_KNOTS ( 'NONE', 3,
 ( #3226, #762, #840, #9060, #10474, #2998, #4427, #2028, #7854, #13005, #15443, #14521, #2426, #3460, #9597, #10707, #6020, #15564 ),
 .UNSPECIFIED., .F., .F.,
 ( 4, 2, 2, 2, 2, 2, 2, 2, 4 ),
 ( 0.003131486019301990727, 0.003522824630466697433, 0.003914163241631404139, 0.004305501852796111278, 0.004696840463960818418, 0.005088179075125524690, 0.005479517686290231830, 0.005870856297454938102, 0.006262194908619645242 ),
 .UNSPECIFIED. ) ;
#12777 = DIRECTION ( 'NONE',  ( 0.000000000000000000, 0.000000000000000000, 1.000000000000000000 ) ) ;
#12778 = FACE_OUTER_BOUND ( 'NONE', #13600, .T. ) ;
#12779 = CARTESIAN_POINT ( 'NONE',  ( -2.639974099233850957, 189.8080084944625128, 8.785674123968128413 ) ) ;
#12780 = SURFACE_STYLE_USAGE ( .BOTH. , #7939 ) ;
#12781 = CARTESIAN_POINT ( 'NONE',  ( 2.662764147438232865, 189.9529664242985518, 5.851057665551680387 ) ) ;
#12782 = CYLINDRICAL_SURFACE ( 'NONE', #10637, 0.9999999999999998890 ) ;
#12783 = DIRECTION ( 'NONE',  ( -1.000000000000000000, 0.000000000000000000, 0.000000000000000000 ) ) ;
#12784 = CARTESIAN_POINT ( 'NONE',  ( 0.5151998000674417044, 228.8897689535086784, 8.809094343595948118 ) ) ;
#12785 = CARTESIAN_POINT ( 'NONE',  ( 5.558508435838229289, -2.857531096718853192, 5.000000000000004441 ) ) ;
#12786 = CARTESIAN_POINT ( 'NONE',  ( -5.726307184802674755, 2.506131700382416394, 4.199734849823247629 ) ) ;
#12787 = CARTESIAN_POINT ( 'NONE',  ( -4.005361199354954493, -4.468319061418810634, 30.19977782616120621 ) ) ;
#12788 = ORIENTED_EDGE ( 'NONE', *, *, #14946, .F. ) ;
#12789 = CARTESIAN_POINT ( 'NONE',  ( -0.8561741729129470624, 188.9999999989074979, 9.066987299999999195 ) ) ;
#12790 = AXIS2_PLACEMENT_3D ( 'NONE', #5800, #8027, #5726 ) ;
#12791 = CARTESIAN_POINT ( 'NONE',  ( -0.8737888311109246464, 5.936248257219519431, 12.00344185141216791 ) ) ;
#12792 = EDGE_CURVE ( 'NONE', #13528, #9302, #13887, .T. ) ;
#12793 = EDGE_LOOP ( 'NONE', ( #4752, #985 ) ) ;
#12794 = CARTESIAN_POINT ( 'NONE',  ( 2.500000000000000444, 184.0000000000000000, 7.000000000000000000 ) ) ;
#12795 = EDGE_CURVE ( 'NONE', #1214, #4630, #2029, .T. ) ;
#12796 = CARTESIAN_POINT ( 'NONE',  ( -1.767766952966369320, 185.9000000000000057, 5.232233047033630235 ) ) ;
#12797 = CARTESIAN_POINT ( 'NONE',  ( -3.634089073485356369, -4.776071126502746900, 5.999920023562623328 ) ) ;
#12798 = CARTESIAN_POINT ( 'NONE',  ( -0.8561741729129452860, 184.6999999989075150, 4.933012699999999029 ) ) ;
#12799 = CARTESIAN_POINT ( 'NONE',  ( 4.344265632482022355, 4.493596842505021449, 17.49574050496990552 ) ) ;
#12800 = CARTESIAN_POINT ( 'NONE',  ( -0.8561741729129456191, 184.4999999989074979, 4.933012699999999029 ) ) ;
#12801 = CARTESIAN_POINT ( 'NONE',  ( -6.176542424588100211, 0.9554180641286806885, 17.99999999999998934 ) ) ;
#12802 = CARTESIAN_POINT ( 'NONE',  ( 1.035533905932739085, -2.500000000000000000, -1.250000000000000222 ) ) ;
#12803 = CARTESIAN_POINT ( 'NONE',  ( -2.500000000000000000, 0.000000000000000000, -1.500000000000000000 ) ) ;
#12804 = CARTESIAN_POINT ( 'NONE',  ( 0.000000000000000000, 229.2449477060184222, 9.834870838912449287 ) ) ;
#12805 = CARTESIAN_POINT ( 'NONE',  ( -2.817313151351109379, -5.579000502529471994, 5.000000000000004441 ) ) ;
#12806 = CARTESIAN_POINT ( 'NONE',  ( -5.782947755040629190, -1.603807858344125092, 17.02601979877759319 ) ) ;
#12807 = CARTESIAN_POINT ( 'NONE',  ( 4.286401442266496886, -4.198423832313229020, 17.99999999999998934 ) ) ;
#12808 = B_SPLINE_CURVE_WITH_KNOTS ( 'NONE', 1,
 ( #4277, #11203 ),
 .UNSPECIFIED., .F., .F.,
 ( 2, 2 ),
 ( 0.000000000000000000, 1.000000000000000000 ),
 .UNSPECIFIED. ) ;
#12809 = EDGE_LOOP ( 'NONE', ( #3584, #12881, #1939, #14316 ) ) ;
#12810 = ORIENTED_EDGE ( 'NONE', *, *, #3396, .F. ) ;
#12811 = VERTEX_POINT ( 'NONE', #9043 ) ;
#12812 = CARTESIAN_POINT ( 'NONE',  ( 4.153440676704390988, -4.671190581744499859, 18.79954462468842280 ) ) ;
#12813 = CARTESIAN_POINT ( 'NONE',  ( 2.449293598294707893E-16, -0.001000000000000132727, -15.50000000000000000 ) ) ;
#12814 = ORIENTED_EDGE ( 'NONE', *, *, #12795, .T. ) ;
#12815 = CARTESIAN_POINT ( 'NONE',  ( -9.750000000000003553, 22.00000000000000000, -3.401296724241641415E-14 ) ) ;
#12816 = CARTESIAN_POINT ( 'NONE',  ( -1.530808498934191571E-16, 2.500000000000000000, 2.184949486963572163E-09 ) ) ;
#12817 = VECTOR ( 'NONE', #6457, 1000.000000000000114 ) ;
#12818 = CARTESIAN_POINT ( 'NONE',  ( -3.882673863916292323, 4.899192824800937096, 31.97408542334170178 ) ) ;
#12819 = CARTESIAN_POINT ( 'NONE',  ( 4.344313232726957352, 4.493553492990258746, 25.00436969680153965 ) ) ;
#12820 = CARTESIAN_POINT ( 'NONE',  ( 1.461580736456473018, 185.3499999989075206, 5.538419263543527649 ) ) ;
#12821 = CARTESIAN_POINT ( 'NONE',  ( 4.592425496802573972E-16, -2.500000000000000000, 1.906999999978150617 ) ) ;
#12822 = CARTESIAN_POINT ( 'NONE',  ( 5.330189595673665792, 2.755293208590188669, 18.26382603205595956 ) ) ;
#12823 = PRODUCT_CONTEXT ( 'NONE', #13696, 'mechanical' ) ;
#12824 = CARTESIAN_POINT ( 'NONE',  ( -2.066987299999999195, -0.8561741729129466183, 1.300000001092474600 ) ) ;
#12825 = CARTESIAN_POINT ( 'NONE',  ( -5.317509234263932072, -2.779225709351048401, 4.869383044678627925 ) ) ;
#12826 = CARTESIAN_POINT ( 'NONE',  ( -1.923824245924939058, 228.4291822535419954, 7.478893683947804405 ) ) ;
#12827 = CARTESIAN_POINT ( 'NONE',  ( 3.159612573729133178, 5.393342049074686173, 18.80026515017675237 ) ) ;
#12828 = EDGE_CURVE ( 'NONE', #11831, #3400, #8384, .T. ) ;
#12829 = ORIENTED_EDGE ( 'NONE', *, *, #15078, .T. ) ;
#12830 = CLOSED_SHELL ( 'NONE', ( #15313, #13856, #6588, #1649, #11389, #9063, #12119, #5629, #14562, #289, #2231, #12314, #5245, #14336, #12929, #3611, #14292, #1320, #2667, #9598, #7008, #4845, #7987, #9833, #10797, #1846, #13407, #3280, #720, #6007 ) ) ;
#12831 = CARTESIAN_POINT ( 'NONE',  ( 4.195842658231538458, -4.289229542213101709, 4.495602393557861731 ) ) ;
#12832 = ORIENTED_EDGE ( 'NONE', *, *, #7884, .F. ) ;
#12833 = CARTESIAN_POINT ( 'NONE',  ( 4.153440676704494905, -4.671190581744405712, 5.799544624688432570 ) ) ;
#12834 = LINE ( 'NONE', #13952, #14996 ) ;
#12835 = CARTESIAN_POINT ( 'NONE',  ( -0.9999502950802086065, 5.916088184763882651, 5.131081491900111757 ) ) ;
#12836 = EDGE_CURVE ( 'NONE', #13014, #8520, #15624, .T. ) ;
#12837 = EDGE_LOOP ( 'NONE', ( #7409, #7488 ) ) ;
#12838 = FACE_OUTER_BOUND ( 'NONE', #4374, .T. ) ;
#12839 = CARTESIAN_POINT ( 'NONE',  ( 1.259047450927248679, 2.184465970885645092, -2.500000000000000444 ) ) ;
#12840 = CARTESIAN_POINT ( 'NONE',  ( 1.500000000000000444, 1.836970198721030427E-16, -5.500000000000000000 ) ) ;
#12841 = CARTESIAN_POINT ( 'NONE',  ( -1.035533905932737753, 2.500000000000000444, -0.8500000000000001998 ) ) ;
#12842 = CARTESIAN_POINT ( 'NONE',  ( 3.010624175977970385, 5.190832888732223260, 4.201117577520603774 ) ) ;
#12843 = DIRECTION ( 'NONE',  ( 0.000000000000000000, 0.000000000000000000, 1.000000000000000000 ) ) ;
#12844 = PRODUCT ( 'connector', 'connector', '', ( #14023 ) ) ;
#12845 = LINE ( 'NONE', #1946, #142 ) ;
#12846 = CARTESIAN_POINT ( 'NONE',  ( -1.035533905932737753, 184.9499999978150413, 4.500000000000000888 ) ) ;
#12847 = CARTESIAN_POINT ( 'NONE',  ( 1.865071889996124055, 228.0459258470066857, 9.553136980667057188 ) ) ;
#12848 = FACE_OUTER_BOUND ( 'NONE', #7485, .T. ) ;
#12849 = CARTESIAN_POINT ( 'NONE',  ( -5.903057025253901635, 1.078199533779546915, 18.61561732698604743 ) ) ;
#12850 = CARTESIAN_POINT ( 'NONE',  ( 2.066987299999999639, 0.8561741729129456191, -0.6999999989075255113 ) ) ;
#12851 = CARTESIAN_POINT ( 'NONE',  ( -6.437450399132682577E-16, 187.0000000000000000, 9.500000000000001776 ) ) ;
#12852 = PLANE ( 'NONE',  #3498 ) ;
#12854 = EDGE_LOOP ( 'NONE', ( #13106, #5616, #13796, #15311 ) ) ;
#12853 = CARTESIAN_POINT ( 'NONE',  ( -0.6156307853267388719, -5.969051238897275624, 25.29870573410680379 ) ) ;
#12855 = CARTESIAN_POINT ( 'NONE',  ( 2.500000000000000444, 185.4999999978150527, 7.000000000000000000 ) ) ;
#12856 = CARTESIAN_POINT ( 'NONE',  ( -5.531623157106110966, 2.327208526676568745, 23.62635295315577011 ) ) ;
#12857 = CARTESIAN_POINT ( 'NONE',  ( -2.057242982682720100, 227.9923142528441815, 9.395475597852444238 ) ) ;
#12858 = CARTESIAN_POINT ( 'NONE',  ( 6.021135683317731413, 1.680226122398092548, 25.47377282875267923 ) ) ;
#12859 = CARTESIAN_POINT ( 'NONE',  ( 1.456896669277396583E-16, 184.1300000002185016, 4.500000000000000000 ) ) ;
#12860 = CYLINDRICAL_SURFACE ( 'NONE', #1691, 1.000000000000000444 ) ;
#12861 = VECTOR ( 'NONE', #9299, 1000.000000000000000 ) ;
#12862 = CARTESIAN_POINT ( 'NONE',  ( 1.862843374206504254, 228.4903663355887318, 7.655596802610238782 ) ) ;
#12863 = DIRECTION ( 'NONE',  ( 0.000000000000000000, 0.000000000000000000, 1.000000000000000000 ) ) ;
#12864 = CARTESIAN_POINT ( 'NONE',  ( -6.021167129161084652, 1.680051667990202446, 4.026404282766995024 ) ) ;
#12865 = CARTESIAN_POINT ( 'NONE',  ( 1.767766952966369320, -1.767766952966368654, 1.300000002184949821 ) ) ;
#12866 = VERTEX_POINT ( 'NONE', #9664 ) ;
#12867 = CARTESIAN_POINT ( 'NONE',  ( 1.461580736456473462, 185.9499999989075150, 5.538419263543526760 ) ) ;
#12868 = PRODUCT_DEFINITION_SHAPE ( 'NONE', 'NONE',  #15768 ) ;
#12869 = CARTESIAN_POINT ( 'NONE',  ( -0.8002302970945894822, 5.947135855825873563, 10.88601773212297985 ) ) ;
#12870 = EDGE_LOOP ( 'NONE', ( #3191, #9347 ) ) ;
#12871 = CARTESIAN_POINT ( 'NONE',  ( -2.668367453516892418, 5.373994336898001656, 24.49999999999999289 ) ) ;
#12872 =( REPRESENTATION_RELATIONSHIP ('NONE','NONE', #11191, #11283 ) REPRESENTATION_RELATIONSHIP_WITH_TRANSFORMATION ( #15542 )SHAPE_REPRESENTATION_RELATIONSHIP( ) );
#12873 = CARTESIAN_POINT ( 'NONE',  ( -4.286401442266532413, -4.198423832313194382, 5.130616955321391615 ) ) ;
#12874 = CARTESIAN_POINT ( 'NONE',  ( -1.035533905932737753, 2.500000000000000444, 0.05000000218494983495 ) ) ;
#12875 = CARTESIAN_POINT ( 'NONE',  ( -2.500000000000000444, 184.0000000000000000, 7.000000000000000000 ) ) ;
#12876 = CARTESIAN_POINT ( 'NONE',  ( -2.066987300000000527, 184.5999999989074922, 6.143825827087054492 ) ) ;
#12877 = CARTESIAN_POINT ( 'NONE',  ( -0.8002720181888681728, 6.199262377003435631, 23.88606262465553343 ) ) ;
#12878 = CARTESIAN_POINT ( 'NONE',  ( 1.035533905932737531, 2.500000000000000444, 0.7500000021849496656 ) ) ;
#12879 = CARTESIAN_POINT ( 'NONE',  ( 2.668367453516645948, -5.373994336898125113, 11.36935038651143515 ) ) ;
#12880 = CARTESIAN_POINT ( 'NONE',  ( 0.000000000000000000, 185.8606548077538321, 9.048340948986950849 ) ) ;
#12881 = ORIENTED_EDGE ( 'NONE', *, *, #11434, .T. ) ;
#12882 = CARTESIAN_POINT ( 'NONE',  ( -2.500000000000000444, 186.8499999999999943, 8.035533905932737753 ) ) ;
#12883 = CARTESIAN_POINT ( 'NONE',  ( -0.8561741729129458411, -2.066987299999999195, -2.399999998907525356 ) ) ;
#12884 = CARTESIAN_POINT ( 'NONE',  ( -0.7988914244716894819, -5.947301735519300969, 17.38456289168617630 ) ) ;
#12885 = ADVANCED_FACE ( 'NONE', ( #9578 ), #14419, .F. ) ;
#12886 = AXIS2_PLACEMENT_3D ( 'NONE', #2376, #8677, #7243 ) ;
#12887 = VERTEX_POINT ( 'NONE', #13233 ) ;
#12888 = ORIENTED_EDGE ( 'NONE', *, *, #14007, .T. ) ;
#12889 = EDGE_LOOP ( 'NONE', ( #10439, #13853 ) ) ;
#12890 = CARTESIAN_POINT ( 'NONE',  ( 3.922396193918953777, -4.541970110199528676, 25.37380682714711000 ) ) ;
#12891 = CARTESIAN_POINT ( 'NONE',  ( 0.000000000000000000, 22.00000000000000000, 0.000000000000000000 ) ) ;
#12892 = ORIENTED_EDGE ( 'NONE', *, *, #4384, .T. ) ;
#12893 = CIRCLE ( 'NONE', #12387, 2.649388036945190095 ) ;
#12894 = CARTESIAN_POINT ( 'NONE',  ( 9.147955830346443662E-17, 185.0000000000000000, 4.500000000000000000 ) ) ;
#12895 = FACE_OUTER_BOUND ( 'NONE', #2903, .T. ) ;
#12897 = EDGE_CURVE ( 'NONE', #9246, #5961, #1212, .T. ) ;
#12896 = AXIS2_PLACEMENT_3D ( 'NONE', #234, #14799, #3884 ) ;
#12898 = CARTESIAN_POINT ( 'NONE',  ( -1.965116437629976787E-16, 189.2499999989075263, 4.933012699999999029 ) ) ;
#12899 = CARTESIAN_POINT ( 'NONE',  ( 2.030576276931546336E-13, 6.000000000000000888, 25.49999999999999645 ) ) ;
#12900 = DIRECTION ( 'NONE',  ( -0.000000000000000000, -1.000000000000000000, -0.000000000000000000 ) ) ;
#12901 = CARTESIAN_POINT ( 'NONE',  ( 1.035533905932738197, 188.5499999978150356, 9.500000000000003553 ) ) ;
#12902 = CARTESIAN_POINT ( 'NONE',  ( 1.035533905932737531, 2.500000000000000444, 0.6569999999781506173 ) ) ;
#12903 =( BOUNDED_CURVE ( )  B_SPLINE_CURVE ( 2, ( #6861, #4462, #2064, #2221, #13209, #3578, #2139, #8370, #873 ),
 .UNSPECIFIED., .F., .F. ) 
 B_SPLINE_CURVE_WITH_KNOTS ( ( 3, 2, 2, 2, 3 ),
 ( 0.2142857142857142738, 0.2321428571428571508, 0.2500000000000000000, 0.2678571428571428492, 0.2857142857142856984 ),
 .UNSPECIFIED. ) 
 CURVE ( )  GEOMETRIC_REPRESENTATION_ITEM ( )  RATIONAL_B_SPLINE_CURVE ( ( 1.000000000000000000, 0.9238795325112867385, 1.000000000000000000, 0.9238795325112867385, 1.000000000000000000, 0.9238795325112867385, 1.000000000000000000, 0.9238795325112867385, 1.000000000000000000 ) ) 
 REPRESENTATION_ITEM ( '' )  );
#12904 = CARTESIAN_POINT ( 'NONE',  ( 1.767766952966369320, 185.5999999978150754, 5.232233047033630235 ) ) ;
#12905 = EDGE_CURVE ( 'NONE', #2808, #13777, #2088, .T. ) ;
#12906 = CARTESIAN_POINT ( 'NONE',  ( -0.8561741729129455081, 2.066987299999999639, 1.900000001092474688 ) ) ;
#12907 = CARTESIAN_POINT ( 'NONE',  ( -1.035533905932739751, 188.5199999975965852, 9.500000000000003553 ) ) ;
#12908 = CARTESIAN_POINT ( 'NONE',  ( -1.104351905119298705, 226.3927175376774699, 4.685770134608635118 ) ) ;
#12909 = CARTESIAN_POINT ( 'NONE',  ( 3.254737477227878983, 5.337033878705280010, 18.87367328635991726 ) ) ;
#12910 = VECTOR ( 'NONE', #5106, 1000.000000000000000 ) ;
#12911 = ORIENTED_EDGE ( 'NONE', *, *, #14182, .T. ) ;
#12912 = CARTESIAN_POINT ( 'NONE',  ( -1.472388569876015740, -2.039937050886111880, -2.501127800403732504 ) ) ;
#12913 = ORIENTED_EDGE ( 'NONE', *, *, #12016, .T. ) ;
#12914 = CARTESIAN_POINT ( 'NONE',  ( -4.416678568553792594, 4.422441866694168944, 17.73763026556123634 ) ) ;
#12915 = CARTESIAN_POINT ( 'NONE',  ( -1.035533905932739751, 189.2499999978150811, 9.500000000000000000 ) ) ;
#12916 = CARTESIAN_POINT ( 'NONE',  ( -0.5039079366032412910, 5.980031194523151683, 4.126370681098134874 ) ) ;
#12917 = ORIENTED_EDGE ( 'NONE', *, *, #639, .T. ) ;
#12918 = EDGE_CURVE ( 'NONE', #9879, #13047, #14941, .T. ) ;
#12919 = CARTESIAN_POINT ( 'NONE',  ( -5.915653884842700272, 1.003805156977486401, 17.49560239355786351 ) ) ;
#12920 = FACE_BOUND ( 'NONE', #430, .T. ) ;
#12921 = CARTESIAN_POINT ( 'NONE',  ( 6.155912734541135301, -1.081577393120877861, 31.50389213124968890 ) ) ;
#12922 = CARTESIAN_POINT ( 'NONE',  ( 2.500000000000000444, -1.035533905932737309, -1.949999999999999956 ) ) ;
#12923 = CARTESIAN_POINT ( 'NONE',  ( -2.668367453516648169, -5.373994336898123336, 31.00000000000000000 ) ) ;
#12924 = PRESENTATION_STYLE_ASSIGNMENT (( #5545 ) ) ;
#12925 = CARTESIAN_POINT ( 'NONE',  ( -1.767766952966369098, 1.767766952966369098, 1.700000002184949732 ) ) ;
#12926 = CARTESIAN_POINT ( 'NONE',  ( -1.767766952966369098, 185.7999999978150356, 5.232233047033630235 ) ) ;
#12927 = CARTESIAN_POINT ( 'NONE',  ( -1.977913707823687250, 228.3348771801055364, 7.206535253053350409 ) ) ;
#12928 = FACE_BOUND ( 'NONE', #6132, .T. ) ;
#12929 = ADVANCED_FACE ( 'NONE', ( #5842 ), #3602, .T. ) ;
#12930 = CARTESIAN_POINT ( 'NONE',  ( -5.866923913994628315, 1.260079467906601858, 18.79952054102714243 ) ) ;
#12931 = CARTESIAN_POINT ( 'NONE',  ( 1.461580736456472573, 1.461580736456472795, -0.6499999989075253559 ) ) ;
#12932 = PRESENTATION_LAYER_ASSIGNMENT (  '', '', ( #2776 ) ) ;
#12933 = CARTESIAN_POINT ( 'NONE',  ( 1.767766952966369098, 188.0999999999999943, 5.232233047033630235 ) ) ;
#12934 = FACE_OUTER_BOUND ( 'NONE', #12349, .T. ) ;
#12935 = EDGE_CURVE ( 'NONE', #2406, #2326, #6236, .T. ) ;
#12937 = ORIENTED_EDGE ( 'NONE', *, *, #13896, .T. ) ;
#12936 = CARTESIAN_POINT ( 'NONE',  ( -13.50000000000000000, 2.000000000000000000, 2.000000000000002220 ) ) ;
#12938 = CARTESIAN_POINT ( 'NONE',  ( -2.500000000000000444, 184.0000000000000000, 7.000000000000000000 ) ) ;
#12939 = CARTESIAN_POINT ( 'NONE',  ( -1.767766952966369320, 186.7000000000000171, 5.232233047033630235 ) ) ;
#12940 = CARTESIAN_POINT ( 'NONE',  ( -1.296916486773226129, 226.4196734319506845, 4.765225606315626194 ) ) ;
#12941 = STYLED_ITEM ( 'NONE', ( #15015 ), #10306 ) ;
#12942 = CARTESIAN_POINT ( 'NONE',  ( 0.07962153170104048494, 190.0874092006666274, 4.202769577405792489 ) ) ;
#12943 = VECTOR ( 'NONE', #14790, 1000.000000000000000 ) ;
#12944 = CYLINDRICAL_SURFACE ( 'NONE', #1474, 1.000000000000000666 ) ;
#12945 = CARTESIAN_POINT ( 'NONE',  ( -1.977662132812563645, 228.3460237620419093, 7.238727217445813267 ) ) ;
#12946 = CARTESIAN_POINT ( 'NONE',  ( 1.620240533814224060, 227.8813442971431016, 5.896706419237646379 ) ) ;
#12947 = FACE_BOUND ( 'NONE', #5844, .T. ) ;
#12948 = CARTESIAN_POINT ( 'NONE',  ( 2.500000000000000000, 3.061616997868383141E-16, 0.6000000021849497545 ) ) ;
#12949 = CARTESIAN_POINT ( 'NONE',  ( -2.782713018890577761, -5.315928322779191362, 30.49560239355785995 ) ) ;
#12950 = VERTEX_POINT ( 'NONE', #896 ) ;
#12951 = CARTESIAN_POINT ( 'NONE',  ( 0.8561741729129457301, 185.9999999989074979, 4.933012699999999029 ) ) ;
#12952 = CARTESIAN_POINT ( 'NONE',  ( -0.8736516769106251745, 5.936271176698245000, 10.99606771578675612 ) ) ;
#12953 = AXIS2_PLACEMENT_3D ( 'NONE', #3616, #8494, #6257 ) ;
#12954 = ORIENTED_EDGE ( 'NONE', *, *, #3313, .T. ) ;
#12955 = CIRCLE ( 'NONE', #6632, 1.499999999999999556 ) ;
#12956 = B_SPLINE_CURVE_WITH_KNOTS ( 'NONE', 3,
 ( #7091, #5896, #10743, #1420, #11136, #8611, #7480, #6222, #236, #4945, #3734, #1346, #10026, #2, #12089, #12246, #13446, #2624 ),
 .UNSPECIFIED., .F., .F.,
 ( 4, 2, 2, 2, 2, 2, 2, 2, 4 ),
 ( 0.000000000000000000, 0.0003914898357794950015, 0.0007829796715589900031, 0.001174469507338485059, 0.001565959343117980006, 0.001957449178897474520, 0.002348939014676968817, 0.002740428850456463113, 0.003131918686235957410 ),
 .UNSPECIFIED. ) ;
#12957 = DIRECTION ( 'NONE',  ( -6.123233995736766036E-17, 1.000000000000000000, 0.000000000000000000 ) ) ;
#12958 = CARTESIAN_POINT ( 'NONE',  ( -1.461580736456473906, 187.1499999989075320, 8.461580736456474128 ) ) ;
#12959 = CARTESIAN_POINT ( 'NONE',  ( 5.935543223013889147, -0.8771126767604598973, 24.36938304467860306 ) ) ;
#12960 = CARTESIAN_POINT ( 'NONE',  ( -1.530808498934191571E-16, 2.500000000000000000, 0.8000000021849498211 ) ) ;
#12961 = CARTESIAN_POINT ( 'NONE',  ( 3.011899281037459630, -5.190111395030252872, 10.69977782616120621 ) ) ;
#12962 = CARTESIAN_POINT ( 'NONE',  ( -1.016439536705160407E-17, 228.2551366889529731, 10.16828399152529272 ) ) ;
#12963 = CARTESIAN_POINT ( 'NONE',  ( -1.530808498934191571E-16, 2.500000000000000000, 0.6999999999999998446 ) ) ;
#12964 = DIRECTION ( 'NONE',  ( 0.000000000000000000, 0.000000000000000000, 1.000000000000000000 ) ) ;
#12965 = DIRECTION ( 'NONE',  ( -0.5877852522924685852, -0.8090169943749508930, 0.000000000000000000 ) ) ;
#12966 = EDGE_LOOP ( 'NONE', ( #1764, #10611, #417, #3122 ) ) ;
#12967 = ORIENTED_EDGE ( 'NONE', *, *, #488, .F. ) ;
#12968 = EDGE_LOOP ( 'NONE', ( #12664, #12489 ) ) ;
#12969 = CARTESIAN_POINT ( 'NONE',  ( 1.461580736456473018, 186.1499999989075320, 5.538419263543527649 ) ) ;
#12970 = CARTESIAN_POINT ( 'NONE',  ( 1.990928271447991671, 228.1755604520575957, 6.746419455620825012 ) ) ;
#12971 = ORIENTED_EDGE ( 'NONE', *, *, #2290, .T. ) ;
#12972 = ADVANCED_FACE ( 'NONE', ( #12985 ), #700, .T. ) ;
#12973 = CARTESIAN_POINT ( 'NONE',  ( 1.035533905932739085, -2.500000000000000000, 1.250000002184949555 ) ) ;
#12974 = CARTESIAN_POINT ( 'NONE',  ( -5.783239563508407954, -1.602707436861167789, 31.97358595436693918 ) ) ;
#12975 = CARTESIAN_POINT ( 'NONE',  ( 4.290381260516126005, 4.545736887716346430, 25.11517780375843145 ) ) ;
#12976 = CARTESIAN_POINT ( 'NONE',  ( 2.066987300000000083, 184.4999999989074979, 6.143825827087054492 ) ) ;
#12977 = CARTESIAN_POINT ( 'NONE',  ( 1.767766952966369320, -1.767766952966368654, -1.993000000021850182 ) ) ;
#12978 = DIRECTION ( 'NONE',  ( 0.5877852522924802425, -0.8090169943749422332, 0.000000000000000000 ) ) ;
#12979 = CONTEXT_DEPENDENT_SHAPE_REPRESENTATION ( #6187, #14403 ) ;
#12980 = CARTESIAN_POINT ( 'NONE',  ( 1.461580736456472573, 1.461580736456472795, 0.1500000010924747995 ) ) ;
#12981 = CARTESIAN_POINT ( 'NONE',  ( -7.386127300057498957E-16, 188.5699999975965397, 9.500000000000001776 ) ) ;
#12982 = CARTESIAN_POINT ( 'NONE',  ( 2.599042177021809508, 227.7726851971488315, 8.749463102108622437 ) ) ;
#12983 = CARTESIAN_POINT ( 'NONE',  ( -0.4907341119409533992, 228.2426455014340263, 10.13156071145469639 ) ) ;
#12984 = VERTEX_POINT ( 'NONE', #3440 ) ;
#12985 = FACE_OUTER_BOUND ( 'NONE', #7700, .T. ) ;
#12986 = ORIENTED_EDGE ( 'NONE', *, *, #2600, .F. ) ;
#12987 = CARTESIAN_POINT ( 'NONE',  ( -4.435347140101170815, 4.403429997944372509, 17.99999999999998934 ) ) ;
#12988 = EDGE_CURVE ( 'NONE', #14887, #14331, #13325, .T. ) ;
#12989 = CARTESIAN_POINT ( 'NONE',  ( -4.322356511625826236, 7.650514973136471220, 11.49999999999998224 ) ) ;
#12990 = CARTESIAN_POINT ( 'NONE',  ( 6.176542424588110869, 0.9554180641286100784, 30.86936067245787996 ) ) ;
#12991 = ORIENTED_EDGE ( 'NONE', *, *, #12708, .T. ) ;
#12992 = EDGE_CURVE ( 'NONE', #11779, #14829, #3076, .T. ) ;
#12993 = CARTESIAN_POINT ( 'NONE',  ( 4.290130679986520867, 4.545972905167775302, 10.88439807107078572 ) ) ;
#12994 = DIRECTION ( 'NONE',  ( 0.000000000000000000, 1.000000000000000000, 0.000000000000000000 ) ) ;
#12995 = VECTOR ( 'NONE', #10620, 1000.000000000000000 ) ;
#12996 = CARTESIAN_POINT ( 'NONE',  ( -3.255128505894364199, 5.336774832660688084, 12.37380055247394672 ) ) ;
#12997 = CARTESIAN_POINT ( 'NONE',  ( -1.035533905932738197, -2.500000000000000000, -2.150000000000000355 ) ) ;
#12998 = CARTESIAN_POINT ( 'NONE',  ( 2.000000000000001776, 0.000000000000000000, 0.000000000000000000 ) ) ;
#12999 = EDGE_CURVE ( 'NONE', #9480, #9099, #4009, .T. ) ;
#13000 = SURFACE_STYLE_FILL_AREA ( #4583 ) ;
#13001 = DIRECTION ( 'NONE',  ( 0.9510565162951500895, 0.3090169943749582204, 0.000000000000000000 ) ) ;
#13002 = PRODUCT ( 'finger', 'finger', '', ( #5604 ) ) ;
#13003 = CARTESIAN_POINT ( 'NONE',  ( 2.500000000000000444, 186.2499999978150527, 8.035533905932739529 ) ) ;
#13004 = CARTESIAN_POINT ( 'NONE',  ( 0.09789622041826544219, 228.2551367208810689, 10.16828408546989237 ) ) ;
#13005 = CARTESIAN_POINT ( 'NONE',  ( 5.903472034603544749, -2.056448723545062585, 16.99991780678442410 ) ) ;
#13006 = ADVANCED_FACE ( 'NONE', ( #12642 ), #9006, .F. ) ;
#13007 = CARTESIAN_POINT ( 'NONE',  ( 0.1306070469495508313, 6.249999999999997335, 23.50000000000000000 ) ) ;
#13008 = B_SPLINE_CURVE_WITH_KNOTS ( 'NONE', 3,
 ( #13334, #12217, #4915, #4754, #13174, #3705, #6191, #8583, #5948, #13413, #2521, #3782, #11029, #15652, #4992, #9843, #14692, #13490, #7449, #12293, #6267, #4674, #2274, #7144, #11980, #1087, #10792, #7683, #8732, #12453, #6660, #7841, #13564, #9921, #10076, #6430, #437, #517, #14774, #1631, #11340, #10157, #11263, #5147, #283, #7526, #1553, #2674, #3860, #14926, #363, #5311, #5387, #12372, #6507, #15011, #1470, #6350, #12688, #8811, #5229, #4017, #5069, #1785, #11184, #4102, #8894, #10001, #11416, #13729, #4179, #15085, #8972, #9050, #13639, #14849, #208, #3935, #12607, #10234, #13876 ),
 .UNSPECIFIED., .F., .F.,
 ( 4, 2, 2, 2, 2, 2, 2, 2, 1, 1, 2, 2, 2, 2, 2, 1, 1, 1, 2, 2, 2, 2, 2, 1, 2, 2, 2, 2, 2, 1, 1, 2, 2, 2, 2, 1, 1, 2, 2, 2, 2, 1, 2, 2, 2, 4 ),
 ( 0.5000594734819727716, 0.5313057563892789048, 0.5469288978429318604, 0.5547404685697585602, 0.5586462539331716881, 0.5625520392965847050, 0.5937983222038856201, 0.6094214636575364663, 0.6172330343843618339, 0.6211388197477740736, 0.6230917124294802489, 0.6250446051111864243, 0.6562908880184755711, 0.6719140294721206441, 0.6797256001989425700, 0.6836313855623541436, 0.6855842782440593197, 0.6865607245849124629, 0.6870489477553389790, 0.6875371709257654951, 0.7187834538332094070, 0.7344065952869320846, 0.7422181660137933124, 0.7461239513772234266, 0.7480768440589389279, 0.7500297367406544291, 0.7812760196480968977, 0.7968991611018190202, 0.8047107318286800259, 0.8086165171921106953, 0.8105694098738263076, 0.8115458562146828925, 0.8125223025555396994, 0.8437685854629449755, 0.8593917269166470030, 0.8672032976434982388, 0.8711090830069236901, 0.8730619756886366378, 0.8750148683703494745, 0.9062611512777616340, 0.9218842927314683244, 0.9296958634583216696, 0.9336016488217482312, 0.9375074341851749038, 0.9687537170925875074, 1.000000000000000000 ),
 .UNSPECIFIED. ) ;
#13009 = CARTESIAN_POINT ( 'NONE',  ( 5.935543223013849179, 0.8771126767607272390, 31.13061695532137918 ) ) ;
#13010 = AXIS2_PLACEMENT_3D ( 'NONE', #11496, #14040, #7765 ) ;
#13011 = CARTESIAN_POINT ( 'NONE',  ( -2.500000000000000888, 187.6500000000000341, 8.035533905932737753 ) ) ;
#13012 = CARTESIAN_POINT ( 'NONE',  ( -4.344502777243695490, 4.493369211529107510, 25.00389213124970667 ) ) ;
#13014 = VERTEX_POINT ( 'NONE', #1663 ) ;
#13013 = CARTESIAN_POINT ( 'NONE',  ( -0.7995298244852583336, -5.947211616899275910, 25.11456014619857413 ) ) ;
#13015 = CARTESIAN_POINT ( 'NONE',  ( -6.105861027178942635, 1.337741388557024624, 18.79954462468841925 ) ) ;
#13016 = EDGE_CURVE ( 'NONE', #3564, #6637, #1972, .T. ) ;
#13017 = DIRECTION ( 'NONE',  ( 0.000000000000000000, 0.000000000000000000, -1.000000000000000000 ) ) ;
#13018 = CARTESIAN_POINT ( 'NONE',  ( -0.9654633820239412190, 226.3742042613716308, 4.631196276447603566 ) ) ;
#13019 = AXIS2_PLACEMENT_3D ( 'NONE', #12675, #12441, #6646 ) ;
#13020 = CARTESIAN_POINT ( 'NONE',  ( 5.859155363331436384, 2.178872204144837621, 25.47400098023329562 ) ) ;
#13021 = CARTESIAN_POINT ( 'NONE',  ( 2.500000000000000444, 185.4800000002184959, 8.035533905932739529 ) ) ;
#13022 = DIRECTION ( 'NONE',  ( -0.000000000000000000, -1.000000000000000000, -0.000000000000000000 ) ) ;
#13023 = CARTESIAN_POINT ( 'NONE',  ( 1.786693786749917301, 227.9723819745098865, 6.159628423921897244 ) ) ;
#13024 = CARTESIAN_POINT ( 'NONE',  ( 6.176542424588117086, 0.9554180641285650033, 11.36936067245785154 ) ) ;
#13025 = DIRECTION ( 'NONE',  ( -0.5877852522924685852, -0.8090169943749508930, 0.000000000000000000 ) ) ;
#13026 = CARTESIAN_POINT ( 'NONE',  ( -2.692215568229745948, -5.362327947133643136, 30.73770962164067200 ) ) ;
#13027 = ORIENTED_EDGE ( 'NONE', *, *, #6399, .T. ) ;
#13028 = CARTESIAN_POINT ( 'NONE',  ( -2.066987300000000971, 185.3999999989075604, 6.143825827087054492 ) ) ;
#13029 = EDGE_CURVE ( 'NONE', #4150, #10768, #10926, .T. ) ;
#13030 = CARTESIAN_POINT ( 'NONE',  ( -0.2622916576875877759, 5.995491482261832594, 12.47384942646812078 ) ) ;
#13031 = ORIENTED_EDGE ( 'NONE', *, *, #6676, .F. ) ;
#13032 = CIRCLE ( 'NONE', #3381, 2.500000000000000000 ) ;
#13033 = CARTESIAN_POINT ( 'NONE',  ( 4.435347140100995844, 4.403429997944549257, 31.00000000000000000 ) ) ;
#13034 = EDGE_CURVE ( 'NONE', #13722, #721, #9085, .T. ) ;
#13035 = CARTESIAN_POINT ( 'NONE',  ( -2.500000000000000000, 0.000000000000000000, 0.2000000021849497878 ) ) ;
#13036 = CARTESIAN_POINT ( 'NONE',  ( -3.061616997868391523E-16, 189.0000000000000000, -7.000000000000000000 ) ) ;
#13037 = CARTESIAN_POINT ( 'NONE',  ( -0.8561741729129458411, 187.6999999989075150, 4.933012699999999029 ) ) ;
#13038 = CARTESIAN_POINT ( 'NONE',  ( 2.692335458626850642, -5.362264153667234190, 18.26239891805596827 ) ) ;
#13039 = CARTESIAN_POINT ( 'NONE',  ( -1.767766952966369098, 1.767766952966369098, -1.499999997815050001 ) ) ;
#13040 = CARTESIAN_POINT ( 'NONE',  ( -6.105861027178951517, -1.337741388556972444, 4.200455375311574535 ) ) ;
#13041 = CARTESIAN_POINT ( 'NONE',  ( -5.999999999999999112, 195.9172377311516016, 6.220370292208425411 ) ) ;
#13042 = CARTESIAN_POINT ( 'NONE',  ( 0.9999505860953618042, -6.169489349035804260, 31.13105903165812194 ) ) ;
#13043 = CARTESIAN_POINT ( 'NONE',  ( -1.461580736456472795, 1.461580736456472795, -2.649999998907524912 ) ) ;
#13044 = VECTOR ( 'NONE', #6998, 1000.000000000000114 ) ;
#13045 = CARTESIAN_POINT ( 'NONE',  ( 5.783198643800769645, 1.602922020054704078, 12.47377823943291375 ) ) ;
#13046 = EDGE_LOOP ( 'NONE', ( #14296, #11541 ) ) ;
#13047 = VERTEX_POINT ( 'NONE', #8925 ) ;
#13048 = ORIENTED_EDGE ( 'NONE', *, *, #13374, .T. ) ;
#13049 = CARTESIAN_POINT ( 'NONE',  ( -4.438452643612533777E-16, 185.0499999989075093, 9.066987300000000971 ) ) ;
#13050 = CARTESIAN_POINT ( 'NONE',  ( 1.582883885363333798, 228.6577406203711575, 8.138983283465440977 ) ) ;
#13051 = EDGE_LOOP ( 'NONE', ( #7738, #10188 ) ) ;
#13052 = CARTESIAN_POINT ( 'NONE',  ( -1.461580736456472795, 1.461580736456472795, 1.950000001092474733 ) ) ;
#13053 = CARTESIAN_POINT ( 'NONE',  ( -0.8736516769104770708, 5.936271176698266316, 23.99606771578674369 ) ) ;
#13054 = LINE ( 'NONE', #9180, #1360 ) ;
#13055 = CARTESIAN_POINT ( 'NONE',  ( 2.500000000000000444, 188.7499999978150527, 5.964466094067262247 ) ) ;
#13056 = CARTESIAN_POINT ( 'NONE',  ( 2.500000000000000000, 3.061616997868383141E-16, 0.5069999999781504840 ) ) ;
#13057 = VECTOR ( 'NONE', #14454, 1000.000000000000114 ) ;
#13058 = CARTESIAN_POINT ( 'NONE',  ( 6.106056299406747101, -1.336851112280680098, 4.201121615766614248 ) ) ;
#13059 = ITEM_DEFINED_TRANSFORMATION ( 'NONE', 'NONE', #10173,  #14201 ) ;
#13060 = CARTESIAN_POINT ( 'NONE',  ( -9.750000000000003553, 22.00000000000000000, 1.499999999999965583 ) ) ;
#13061 = CARTESIAN_POINT ( 'NONE',  ( 2.996417732210646889, -5.485687819086863648, 4.386038205919295940 ) ) ;
#13062 = CARTESIAN_POINT ( 'NONE',  ( 2.692585213447247661, 226.8629897650803855, 6.071564533969844746 ) ) ;
#13063 = DIRECTION ( 'NONE',  ( 0.000000000000000000, 0.000000000000000000, 1.000000000000000000 ) ) ;
#13064 = ORIENTED_EDGE ( 'NONE', *, *, #1934, .F. ) ;
#13065 = DIRECTION ( 'NONE',  ( 0.000000000000000000, 0.000000000000000000, -1.000000000000000000 ) ) ;
#13066 = ORIENTED_EDGE ( 'NONE', *, *, #3180, .T. ) ;
#13067 = ORIENTED_EDGE ( 'NONE', *, *, #12905, .F. ) ;
#13068 = CARTESIAN_POINT ( 'NONE',  ( 2.094888806938587637E-14, 6.250000000000000888, 30.00000000000000000 ) ) ;
#13069 = AXIS2_PLACEMENT_3D ( 'NONE', #4127, #12634, #5569 ) ;
#13070 = CARTESIAN_POINT ( 'NONE',  ( -3.634089073485525123, -4.776071126502616337, 25.49992002356260912 ) ) ;
#13071 = ORIENTED_EDGE ( 'NONE', *, *, #534, .T. ) ;
#13072 = CARTESIAN_POINT ( 'NONE',  ( 2.500000000000000000, 3.061616997868383141E-16, 2.500000000000000000 ) ) ;
#13073 = CARTESIAN_POINT ( 'NONE',  ( 0.000000000000000000, 0.000000000000000000, 2.500000000000000000 ) ) ;
#13074 = CARTESIAN_POINT ( 'NONE',  ( -0.5030929395818275474, -6.230885867001161316, 23.62600319116548775 ) ) ;
#13075 = CARTESIAN_POINT ( 'NONE',  ( -3.781065399486035261, -4.978303713186424950, 18.99991741810288559 ) ) ;
#13076 = CARTESIAN_POINT ( 'NONE',  ( 1.353717517954364224E-13, -6.000000000000000888, 18.99999999999998934 ) ) ;
#13077 = CARTESIAN_POINT ( 'NONE',  ( 0.000000000000000000, 2.000000000000000000, 0.000000000000000000 ) ) ;
#13078 =( NAMED_UNIT ( * ) PLANE_ANGLE_UNIT ( ) SI_UNIT ( $, .RADIAN. ) );
#13079 = CARTESIAN_POINT ( 'NONE',  ( 5.317509234263932072, 2.779225709351047957, 5.132360785839114925 ) ) ;
#13080 = CARTESIAN_POINT ( 'NONE',  ( -1.524659305057740610E-16, 189.0000000000000000, 4.500000000000000000 ) ) ;
#13081 = ADVANCED_FACE ( 'NONE', ( #6383, #7715 ), #242, .F. ) ;
#13082 = CARTESIAN_POINT ( 'NONE',  ( 1.057043591443594943, 228.1937260751906820, 9.987734910156856216 ) ) ;
#13083 = CIRCLE ( 'NONE', #8545, 2.000000000000000000 ) ;
#13084 = CARTESIAN_POINT ( 'NONE',  ( -6.021167129161020704, -1.680051667990425379, 18.97359571723300320 ) ) ;
#13085 = EDGE_CURVE ( 'NONE', #5746, #6892, #13758, .T. ) ;
#13086 = CARTESIAN_POINT ( 'NONE',  ( -9.750000000000003553, 184.0000000000000000, -1.500000000000033751 ) ) ;
#13087 = ORIENTED_EDGE ( 'NONE', *, *, #5524, .T. ) ;
#13088 = LINE ( 'NONE', #6107, #6832 ) ;
#13089 = EDGE_CURVE ( 'NONE', #5348, #14086, #8085, .T. ) ;
#13090 = CARTESIAN_POINT ( 'NONE',  ( 0.9735856429313511917, -5.920699391845015924, 11.76285283906725354 ) ) ;
#13092 = ORIENTED_EDGE ( 'NONE', *, *, #2206, .F. ) ;
#13091 = CARTESIAN_POINT ( 'NONE',  ( -0.7988914244716200930, -5.947301735519313404, 23.88456289168616919 ) ) ;
#13093 = DIRECTION ( 'NONE',  ( 0.000000000000000000, 1.000000000000000000, 0.000000000000000000 ) ) ;
#13094 = CYLINDRICAL_SURFACE ( 'NONE', #772, 1.000000000000000888 ) ;
#13095 = ORIENTED_EDGE ( 'NONE', *, *, #11539, .F. ) ;
#13096 = CARTESIAN_POINT ( 'NONE',  ( -5.935543223013830527, 0.8771126767608677932, 24.36760611998364823 ) ) ;
#13097 = CARTESIAN_POINT ( 'NONE',  ( -2.272721100113404447, 226.6597439602984139, 5.472753651262165064 ) ) ;
#13098 = CARTESIAN_POINT ( 'NONE',  ( 0.2845864031260020854, 190.0868499456632605, 4.208331950485010964 ) ) ;
#13099 = CARTESIAN_POINT ( 'NONE',  ( 1.767766952966368654, 184.6300000002185016, 8.767766952966368876 ) ) ;
#13100 = LINE ( 'NONE', #8345, #11607 ) ;
#13101 = CARTESIAN_POINT ( 'NONE',  ( 0.4540882845019501568, 227.6260587419843091, 5.159427175404782240 ) ) ;
#13102 = EDGE_CURVE ( 'NONE', #2089, #902, #7256, .T. ) ;
#13103 = FACE_BOUND ( 'NONE', #1442, .T. ) ;
#13104 = CARTESIAN_POINT ( 'NONE',  ( -1.461580736456472795, 1.461580736456472795, 0.5500000010924748217 ) ) ;
#13105 = CARTESIAN_POINT ( 'NONE',  ( -3.420659742068319353, -4.931142898501779115, 30.00004946353777058 ) ) ;
#13106 = ORIENTED_EDGE ( 'NONE', *, *, #1079, .F. ) ;
#13107 = CARTESIAN_POINT ( 'NONE',  ( -5.793705359219414319E-16, 187.2499999989075263, 9.066987300000000971 ) ) ;
#13108 = CARTESIAN_POINT ( 'NONE',  ( -0.5044069930202613739, 5.979990686695000335, 12.37335743227902718 ) ) ;
#13109 = ORIENTED_EDGE ( 'NONE', *, *, #3396, .T. ) ;
#13110 = DIRECTION ( 'NONE',  ( -1.062480551894329776E-17, -2.775557561562888393E-16, 1.000000000000000000 ) ) ;
#13111 = DIRECTION ( 'NONE',  ( 1.000000000000000000, 0.000000000000000000, 0.000000000000000000 ) ) ;
#13112 = CIRCLE ( 'NONE', #15162, 1.500000000000000000 ) ;
#13113 = CARTESIAN_POINT ( 'NONE',  ( 5.746619684944291429, 1.730157667110781672, 16.99995067926686687 ) ) ;
#13114 = CARTESIAN_POINT ( 'NONE',  ( 2.066987300000000527, 185.8999999989075320, 6.143825827087054492 ) ) ;
#13115 = CARTESIAN_POINT ( 'NONE',  ( 4.286401442266437378, 4.198423832313292969, 18.13239388001634467 ) ) ;
#13116 = CARTESIAN_POINT ( 'NONE',  ( -1.035533905932737753, 2.500000000000000444, -1.549999997815050268 ) ) ;
#13117 = CARTESIAN_POINT ( 'NONE',  ( -6.176542424588105540, -0.9554180641286327269, 5.000000000000004441 ) ) ;
#13118 = CARTESIAN_POINT ( 'NONE',  ( -5.999999999999999112, 222.7460571280668091, 12.08513476933103448 ) ) ;
#13119 = CARTESIAN_POINT ( 'NONE',  ( 4.322356511625595310, 7.650514973136599117, 11.49999999999998224 ) ) ;
#13120 = CARTESIAN_POINT ( 'NONE',  ( -5.387129544537350156E-16, 185.2999999978150356, 9.500000000000001776 ) ) ;
#13121 = CYLINDRICAL_SURFACE ( 'NONE', #3633, 0.9999999999999998890 ) ;
#13122 = ORIENTED_EDGE ( 'NONE', *, *, #5703, .F. ) ;
#13123 = EDGE_CURVE ( 'NONE', #15509, #8237, #1213, .T. ) ;
#13124 = ORIENTED_EDGE ( 'NONE', *, *, #9282, .T. ) ;
#13125 = PRODUCT_RELATED_PRODUCT_CATEGORY ( 'part', '', ( #2311 ) ) ;
#13126 = ORIENTED_EDGE ( 'NONE', *, *, #7594, .F. ) ;
#13127 = CARTESIAN_POINT ( 'NONE',  ( -0.8561741729129455081, 184.6999999989075150, 4.933012699999999029 ) ) ;
#13128 = CARTESIAN_POINT ( 'NONE',  ( 0.1295330668958723785, 227.6089706593652693, 5.110075818160935590 ) ) ;
#13129 = ADVANCED_FACE ( 'NONE', ( #5263 ), #6820, .T. ) ;
#13130 = ORIENTED_EDGE ( 'NONE', *, *, #13196, .T. ) ;
#13131 = PRODUCT_DEFINITION_SHAPE ( 'NONE', 'NONE',  #15741 ) ;
#13132 = CARTESIAN_POINT ( 'NONE',  ( -2.500000000000000000, -1.035533905932739307, -2.949999997815051067 ) ) ;
#13133 = CARTESIAN_POINT ( 'NONE',  ( -5.842945980534652861, -1.369128644668926809, 31.87378430870261425 ) ) ;
#13134 = AXIS2_PLACEMENT_3D ( 'NONE', #14691, #9771, #14528 ) ;
#13135 = CARTESIAN_POINT ( 'NONE',  ( 3.883716939928917977, 4.898343590941304448, 25.47359571723300675 ) ) ;
#13136 = CARTESIAN_POINT ( 'NONE',  ( 2.066987300000000083, 186.8499999989075206, 7.000000000000000000 ) ) ;
#13137 = CARTESIAN_POINT ( 'NONE',  ( -1.035533905932737753, 2.500000000000000444, -0.8430000000218496048 ) ) ;
#13138 = CARTESIAN_POINT ( 'NONE',  ( 6.081836621194441683, -1.445163676684824594, 4.126941084456995590 ) ) ;
#13139 = CARTESIAN_POINT ( 'NONE',  ( 3.796994071234844259E-16, -2.066987299999999639, -0.1499999989075253282 ) ) ;
#13140 = CARTESIAN_POINT ( 'NONE',  ( 3.568242062701607598, -5.132954954975453177, 3.999950931234679263 ) ) ;
#13141 = CARTESIAN_POINT ( 'NONE',  ( 2.691218579993890803, 227.7172414894967858, 8.586351398698511161 ) ) ;
#13142 = CARTESIAN_POINT ( 'NONE',  ( 4.286401442266518202, 4.198423832313208592, 31.00000000000000000 ) ) ;
#13143 = ORIENTED_EDGE ( 'NONE', *, *, #14842, .F. ) ;
#13144 = ORIENTED_EDGE ( 'NONE', *, *, #1143, .F. ) ;
#13145 = CARTESIAN_POINT ( 'NONE',  ( 2.692143549875480435, -5.362363179736437502, 4.738056759968539922 ) ) ;
#13146 = AXIS2_PLACEMENT_3D ( 'NONE', #9785, #13433, #3799 ) ;
#13147 = ORIENTED_EDGE ( 'NONE', *, *, #8639, .F. ) ;
#13148 = ORIENTED_EDGE ( 'NONE', *, *, #13975, .T. ) ;
#13149 = CARTESIAN_POINT ( 'NONE',  ( 0.6144300524833891108, 6.220417338033052523, 30.20033372175935327 ) ) ;
#13150 = AXIS2_PLACEMENT_3D ( 'NONE', #1986, #4541, #5894 ) ;
#13151 = CARTESIAN_POINT ( 'NONE',  ( 3.107278289587155573, -5.134157760522071179, 17.12635295315575235 ) ) ;
#13152 = CARTESIAN_POINT ( 'NONE',  ( 0.7993401192311868630, -6.199366368793663540, 5.614832469365748757 ) ) ;
#13153 = ORIENTED_EDGE ( 'NONE', *, *, #2168, .F. ) ;
#13154 = CARTESIAN_POINT ( 'NONE',  ( -5.317509234263906315, 2.779225709351095475, 17.99999999999998934 ) ) ;
#13155 = UNCERTAINTY_MEASURE_WITH_UNIT (LENGTH_MEASURE( 1.000000000000000082E-05 ), #538, 'distance_accuracy_value', 'NONE');
#13156 = CARTESIAN_POINT ( 'NONE',  ( 2.668367453516444776, 5.373994336898222812, 24.49999999999999289 ) ) ;
#13157 = FACE_BOUND ( 'NONE', #7599, .T. ) ;
#13158 = CARTESIAN_POINT ( 'NONE',  ( -1.767766952966368432, -1.767766952966369320, -1.299999997815050490 ) ) ;
#13159 = CARTESIAN_POINT ( 'NONE',  ( 5.409274167810628420, 2.597759609440700057, 30.38480617551148910 ) ) ;
#13160 = CYLINDRICAL_SURFACE ( 'NONE', #5667, 0.9999999999999998890 ) ;
#13161 = CARTESIAN_POINT ( 'NONE',  ( 0.000000000000000000, 0.000000000000000000, 0.000000000000000000 ) ) ;
#13162 = CIRCLE ( 'NONE', #2747, 12.50000000000000533 ) ;
#13163 = CARTESIAN_POINT ( 'NONE',  ( 1.767766952966369098, 187.1999999978150697, 5.232233047033630235 ) ) ;
#13164 = CARTESIAN_POINT ( 'NONE',  ( 0.6804430692981219275, 228.2300923459994237, 10.09465452691961751 ) ) ;
#13165 = CARTESIAN_POINT ( 'NONE',  ( 3.107278289587176445, 5.134157760522058744, 31.87364704684422634 ) ) ;
#13166 = CARTESIAN_POINT ( 'NONE',  ( -1.170841281832480263, 188.9999999981235703, 4.783420672645316785 ) ) ;
#13167 = ORIENTED_EDGE ( 'NONE', *, *, #5722, .T. ) ;
#13168 = CARTESIAN_POINT ( 'NONE',  ( -5.842988226680567720, 1.369004370660693137, 12.37380682714709756 ) ) ;
#13169 = CARTESIAN_POINT ( 'NONE',  ( -0.5042987395406965945, -5.979983180450083147, 12.37329304179975509 ) ) ;
#13170 = CIRCLE ( 'NONE', #464, 6.000000000000000888 ) ;
#13172 = VERTEX_POINT ( 'NONE', #11686 ) ;
#13171 = CARTESIAN_POINT ( 'NONE',  ( 2.500000000000000000, 187.9500000000000455, 8.035533905932739529 ) ) ;
#13173 = DIRECTION ( 'NONE',  ( -0.000000000000000000, -1.000000000000000000, -0.000000000000000000 ) ) ;
#13174 = CARTESIAN_POINT ( 'NONE',  ( 0.7722673575711334060, 226.3571150073143770, 4.580780788055321295 ) ) ;
#13175 = EDGE_LOOP ( 'NONE', ( #7791, #5558, #532, #14236 ) ) ;
#13176 = CARTESIAN_POINT ( 'NONE',  ( -5.782947755040658500, -1.603807858344011406, 30.02601979877761096 ) ) ;
#13177 = EDGE_CURVE ( 'NONE', #10924, #398, #3247, .T. ) ;
#13178 = CARTESIAN_POINT ( 'NONE',  ( 1.461580736456473018, -1.461580736456472573, 1.750000001092474999 ) ) ;
#13179 = CARTESIAN_POINT ( 'NONE',  ( -2.826874103312618569, 227.6159703306986444, 8.288388193239365265 ) ) ;
#13180 = FILL_AREA_STYLE_COLOUR ( '', #6092 ) ;
#13181 = CARTESIAN_POINT ( 'NONE',  ( -5.769755079862307845, 2.405651898699003421, 12.37305891554298931 ) ) ;
#13182 = CARTESIAN_POINT ( 'NONE',  ( -6.877907531704918753E-16, 187.7300000002184959, 9.500000000000001776 ) ) ;
#13183 = CARTESIAN_POINT ( 'NONE',  ( -2.841041022017386286, 5.567186575787263614, 5.262252817217141221 ) ) ;
#13184 = APPLICATION_CONTEXT ( 'automotive_design' ) ;
#13185 = CARTESIAN_POINT ( 'NONE',  ( -0.1316767729515891938, 227.6100531710845587, 5.113202173749356483 ) ) ;
#13187 = LINE ( 'NONE', #14539, #14607 ) ;
#13186 = AXIS2_PLACEMENT_3D ( 'NONE', #12739, #1841, #2968 ) ;
#13188 = CARTESIAN_POINT ( 'NONE',  ( -0.8561741729129455081, 2.066987299999999639, 1.300000001092475044 ) ) ;
#13189 = DIRECTION ( 'NONE',  ( -6.123233995736766036E-17, 1.000000000000000000, 0.000000000000000000 ) ) ;
#13190 = EDGE_LOOP ( 'NONE', ( #10616, #14421 ) ) ;
#13191 = CARTESIAN_POINT ( 'NONE',  ( 0.8561741729129458411, 188.8999999989074752, 9.066987300000000971 ) ) ;
#13192 = CARTESIAN_POINT ( 'NONE',  ( 2.066987300000000083, 186.5999999989074922, 7.856174172912946396 ) ) ;
#13193 = FACE_OUTER_BOUND ( 'NONE', #5105, .T. ) ;
#13194 = ORIENTED_EDGE ( 'NONE', *, *, #10709, .F. ) ;
#13195 = CARTESIAN_POINT ( 'NONE',  ( -3.011139120916454637, -5.190534000030377904, 4.200681937418262457 ) ) ;
#13196 = EDGE_CURVE ( 'NONE', #567, #12426, #3429, .T. ) ;
#13197 = PRESENTATION_LAYER_ASSIGNMENT (  '', '', ( #14459 ) ) ;
#13198 = CARTESIAN_POINT ( 'NONE',  ( 5.843075991566581529, -1.368655265451063086, 5.873647046844242325 ) ) ;
#13199 = B_SPLINE_CURVE_WITH_KNOTS ( 'NONE', 3,
 ( #7646, #774, #4360, #3977, #5187, #5562, #2796, #2717, #12337, #13765, #15258, #12417, #3899, #12494, #2874, #1962, #327, #13605, #1593, #14054, #6391, #5637, #12779, #10487, #7938, #9293, #1883, #11590, #6471, #6758, #11304, #10119, #11148, #14891 ),
 .UNSPECIFIED., .F., .F.,
 ( 4, 2, 2, 2, 2, 2, 2, 2, 2, 2, 2, 2, 2, 2, 2, 2, 4 ),
 ( 0.009569887493644234008, 0.01016303449442789927, 0.01075618149521156454, 0.01134932849599522980, 0.01194247549677889680, 0.01253562249756256207, 0.01312876949834622733, 0.01372191649912989260, 0.01431506349991355787, 0.01490821050069722487, 0.01550135750148089187, 0.01609450450226455887, 0.01668765150304822587, 0.01728079850383189287, 0.01787394550461555986, 0.01846709250539923033, 0.01906023950618289733 ),
 .UNSPECIFIED. ) ;
#13200 = VECTOR ( 'NONE', #514, 1000.000000000000114 ) ;
#13201 = FACE_BOUND ( 'NONE', #14527, .T. ) ;
#13202 = CARTESIAN_POINT ( 'NONE',  ( 0.7988860301923105256, 6.199427171881326082, 10.88455580536195377 ) ) ;
#13203 = CARTESIAN_POINT ( 'NONE',  ( -0.8561741729129470624, 187.1999999989075434, 9.066987300000000971 ) ) ;
#13204 = B_SPLINE_CURVE_WITH_KNOTS ( 'NONE', 3,
 ( #7446, #2751, #8807, #8891, #8968, #12290, #10073, #4014, #5065, #14771, #5384, #6345, #13636, #6578, #10153, #9998, #7679, #11412 ),
 .UNSPECIFIED., .F., .F.,
 ( 4, 2, 2, 2, 2, 2, 2, 2, 4 ),
 ( 0.000000000000000000, 0.0003914357524127465640, 0.0007828715048254931280, 0.001174307257238239692, 0.001565743009650986256, 0.001957178762063731519, 0.002348614514476477216, 0.002740050266889222479, 0.003131486019301968175 ),
 .UNSPECIFIED. ) ;
#13205 = CARTESIAN_POINT ( 'NONE',  ( 2.782156709077369339, -5.316215864844073380, 18.50312048902377526 ) ) ;
#13206 = CARTESIAN_POINT ( 'NONE',  ( -1.530808498934191571E-16, 2.500000000000000000, 2.184949703804006660E-09 ) ) ;
#13207 = CARTESIAN_POINT ( 'NONE',  ( 3.421280866381160024, -4.930711975950901937, 10.49995067926686687 ) ) ;
#13208 = CARTESIAN_POINT ( 'NONE',  ( 5.329945432499622271, -2.755769831645151324, 31.26229037835932090 ) ) ;
#13209 = CARTESIAN_POINT ( 'NONE',  ( 4.592425496802573972E-16, -2.500000000000000000, 1.100000000000000089 ) ) ;
#13210 = CARTESIAN_POINT ( 'NONE',  ( 5.329945432499570757, 2.755769831645247692, 4.737709621640687985 ) ) ;
#13211 = CARTESIAN_POINT ( 'NONE',  ( 5.487097279078438028, 2.429065649168800523, 12.29952054102714243 ) ) ;
#13212 = ORIENTED_EDGE ( 'NONE', *, *, #4476, .F. ) ;
#13213 = STYLED_ITEM ( 'NONE', ( #521 ), #7656 ) ;
#13214 = VERTEX_POINT ( 'NONE', #8031 ) ;
#13215 = ORIENTED_EDGE ( 'NONE', *, *, #12792, .T. ) ;
#13216 = CARTESIAN_POINT ( 'NONE',  ( -2.940898392866930777E-15, 228.9118723800512498, 8.872930300147352511 ) ) ;
#13217 = ORIENTED_EDGE ( 'NONE', *, *, #1324, .T. ) ;
#13218 = CARTESIAN_POINT ( 'NONE',  ( -1.035533905932738197, -2.500000000000000000, -2.849999997815050978 ) ) ;
#13219 = CARTESIAN_POINT ( 'NONE',  ( -5.531623157106149158, -2.327208526676475930, 31.87364704684421923 ) ) ;
#13220 = DIRECTION ( 'NONE',  ( 0.000000000000000000, 0.000000000000000000, 1.000000000000000000 ) ) ;
#13221 = CARTESIAN_POINT ( 'NONE',  ( -1.016439536705160407E-17, 186.2499999989074979, 4.933012699999999029 ) ) ;
#13222 = EDGE_CURVE ( 'NONE', #8130, #13429, #6500, .T. ) ;
#13223 = CARTESIAN_POINT ( 'NONE',  ( 2.500000000000000444, 1.035533905932737975, -0.2430000000218497103 ) ) ;
#13224 = CARTESIAN_POINT ( 'NONE',  ( -5.531209434046356677, 2.328189801702577277, 31.87303779027051576 ) ) ;
#13225 = ITEM_DEFINED_TRANSFORMATION ( 'NONE', 'NONE', #4841,  #14201 ) ;
#13226 = CARTESIAN_POINT ( 'NONE',  ( 3.796994071234844259E-16, -2.066987299999999639, 1.650000001092474911 ) ) ;
#13227 = CARTESIAN_POINT ( 'NONE',  ( 4.069684453406360092, -4.744965295353502199, 30.12619944752604439 ) ) ;
#13228 = CARTESIAN_POINT ( 'NONE',  ( 1.501755279530002651, 226.4544816774725575, 4.867834892302488115 ) ) ;
#13229 = DIRECTION ( 'NONE',  ( -1.062480551894329930E-17, -2.775557561562888393E-16, 1.000000000000000000 ) ) ;
#13230 = EDGE_LOOP ( 'NONE', ( #12021, #2286, #1154, #4953 ) ) ;
#13231 = B_SPLINE_CURVE_WITH_KNOTS ( 'NONE', 3,
 ( #14513, #6175, #11089, #3689, #8489, #6011, #1068, #10853, #15719, #13317, #7286, #34, #4899, #7127, #8567, #7360, #11012, #14344 ),
 .UNSPECIFIED., .F., .F.,
 ( 4, 2, 2, 2, 2, 2, 2, 2, 4 ),
 ( 0.003131918686235948303, 0.003523310662250241174, 0.003914702638264534046, 0.004306094614278826484, 0.004697486590293120656, 0.005088878566307413961, 0.005480270542321708134, 0.005871662518336002307, 0.006263054494350295612 ),
 .UNSPECIFIED. ) ;
#13232 = VERTEX_POINT ( 'NONE', #4610 ) ;
#13233 = CARTESIAN_POINT ( 'NONE',  ( -2.500000000000000000, 0.000000000000000000, 0.09999999999999982514 ) ) ;
#13234 = EDGE_LOOP ( 'NONE', ( #10746, #10109, #11445, #11776 ) ) ;
#13235 = ORIENTED_EDGE ( 'NONE', *, *, #10297, .F. ) ;
#13236 = CARTESIAN_POINT ( 'NONE',  ( -5.984759433606971157, 1.806271833852423070, 25.50008219321556524 ) ) ;
#13237 = CARTESIAN_POINT ( 'NONE',  ( -4.416837305303585204, -4.422286678978921692, 24.23809786915986919 ) ) ;
#13238 = CARTESIAN_POINT ( 'NONE',  ( 0.2622538972264162327, -6.245673238944476680, 5.973859943692001906 ) ) ;
#13239 = CARTESIAN_POINT ( 'NONE',  ( -5.726307184802632122, -2.506131700382510985, 31.80026515017676658 ) ) ;
#13240 = CARTESIAN_POINT ( 'NONE',  ( -0.1306070469493368635, -6.249999999999999112, 4.000000000000003553 ) ) ;
#13241 = DIRECTION ( 'NONE',  ( 0.000000000000000000, -0.000000000000000000, 1.000000000000000000 ) ) ;
#13242 = CARTESIAN_POINT ( 'NONE',  ( -4.416837305303549677, 4.422286678978957219, 11.76190213084010239 ) ) ;
#13243 = CARTESIAN_POINT ( 'NONE',  ( -5.984759433606947177, -1.806271833852501674, 23.49991780678443476 ) ) ;
#13244 = CARTESIAN_POINT ( 'NONE',  ( -2.782769401326143477, -5.315896561274865206, 31.50428920362020335 ) ) ;
#13245 = DIRECTION ( 'NONE',  ( 6.982962677686266711E-15, 0.000000000000000000, -1.000000000000000000 ) ) ;
#13246 = CARTESIAN_POINT ( 'NONE',  ( 1.035533905932738197, 186.9499999978150413, 9.500000000000003553 ) ) ;
#13247 = CARTESIAN_POINT ( 'NONE',  ( 0.4902782441471901231, 226.3376063806459513, 4.523301387120397088 ) ) ;
#13248 = CARTESIAN_POINT ( 'NONE',  ( 0.000000000000000000, 0.000000000000000000, 5.000000000000004441 ) ) ;
#13249 = CARTESIAN_POINT ( 'NONE',  ( -0.2987180493634195022, 188.9999999992114397, 4.511177095514812940 ) ) ;
#13250 = EDGE_LOOP ( 'NONE', ( #2192, #4689, #12788, #10457 ) ) ;
#13251 = CARTESIAN_POINT ( 'NONE',  ( 4.435347140100914132, 4.403429997944631857, 17.99999999999998934 ) ) ;
#13252 = B_SPLINE_CURVE_WITH_KNOTS ( 'NONE', 3,
 ( #7736, #12584, #6169, #8637, #14672, #13469, #7428, #4314, #6556, #14164, #15373, #5594, #15137, #571, #1916, #15214, #804, #496 ),
 .UNSPECIFIED., .F., .F.,
 ( 4, 2, 2, 2, 2, 2, 2, 2, 4 ),
 ( 0.003131486019302004171, 0.003522824630466709142, 0.003914163241631414547, 0.004305501852796119085, 0.004696840463960824490, 0.005088179075125529027, 0.005479517686290234432, 0.005870856297454939837, 0.006262194908619644375 ),
 .UNSPECIFIED. ) ;
#13253 = DIRECTION ( 'NONE',  ( 1.000000000000000000, 0.000000000000000000, 0.000000000000000000 ) ) ;
#13255 = ORIENTED_EDGE ( 'NONE', *, *, #10846, .T. ) ;
#13254 = DIRECTION ( 'NONE',  ( 0.000000000000000000, -1.000000000000000000, 0.000000000000000000 ) ) ;
#13256 = CARTESIAN_POINT ( 'NONE',  ( 0.01615993435121231697, -0.3999999999999993006, 2.507354378531367889 ) ) ;
#13257 = AXIS2_PLACEMENT_3D ( 'NONE', #9964, #12260, #11070 ) ;
#13258 = PLANE ( 'NONE',  #9938 ) ;
#13259 = LINE ( 'NONE', #13415, #3094 ) ;
#13260 = CARTESIAN_POINT ( 'NONE',  ( 2.066987299999999639, 0.8561741729129456191, 1.100000001092475088 ) ) ;
#13261 = CARTESIAN_POINT ( 'NONE',  ( -0.7719220162881343938, 226.3554759578498476, 4.575941956958391899 ) ) ;
#13262 = CARTESIAN_POINT ( 'NONE',  ( -0.9740012993919970885, -6.173846968979643357, 31.26164920628438892 ) ) ;
#13263 = CARTESIAN_POINT ( 'NONE',  ( 2.500000000000000444, 187.0800000002184618, 8.035533905932739529 ) ) ;
#13264 = LINE ( 'NONE', #929, #8831 ) ;
#13265 = CARTESIAN_POINT ( 'NONE',  ( 0.06504883222449296676, 227.6089665442046339, 5.110063933342379627 ) ) ;
#13266 = CARTESIAN_POINT ( 'NONE',  ( 1.813601955701626300, 228.5298646585827385, 7.769670212251800656 ) ) ;
#13267 = CARTESIAN_POINT ( 'NONE',  ( 1.461580736456473018, -1.461580736456472573, -0.6499999989075253559 ) ) ;
#13268 = VECTOR ( 'NONE', #3300, 1000.000000000000227 ) ;
#13269 = CARTESIAN_POINT ( 'NONE',  ( 2.500000000000000000, 3.061616997868383141E-16, 1.300000000000000044 ) ) ;
#13270 = ORIENTED_EDGE ( 'NONE', *, *, #14566, .T. ) ;
#13271 = CARTESIAN_POINT ( 'NONE',  ( -9.750000000000003553, 19.99999999999999645, -3.401296724241641415E-14 ) ) ;
#13272 = CARTESIAN_POINT ( 'NONE',  ( 0.8561741729129460632, 187.2999999989075661, 9.066987300000000971 ) ) ;
#13273 = CARTESIAN_POINT ( 'NONE',  ( 6.780834062235653815E-14, 6.000000000000000888, 10.49999999999998224 ) ) ;
#13274 = ORIENTED_EDGE ( 'NONE', *, *, #11675, .T. ) ;
#13275 = CARTESIAN_POINT ( 'NONE',  ( -2.668367453516814258, -5.373994336898041624, 24.36760611998364467 ) ) ;
#13276 = DIRECTION ( 'NONE',  ( 1.062480551894329776E-17, 2.775557561562888393E-16, -1.000000000000000000 ) ) ;
#13277 = AXIS2_PLACEMENT_3D ( 'NONE', #10681, #15303, #15617 ) ;
#13278 = FILL_AREA_STYLE_COLOUR ( '', #12537 ) ;
#13279 = CARTESIAN_POINT ( 'NONE',  ( 0.5042675786779380331, 6.230788509548837339, 12.37331068310448678 ) ) ;
#13280 = CARTESIAN_POINT ( 'NONE',  ( 1.461580736456472573, 186.5499999989075093, 8.461580736456474128 ) ) ;
#13281 = CARTESIAN_POINT ( 'NONE',  ( 3.633127580202223150, -4.776802569231096030, 19.00007961174475213 ) ) ;
#13282 = CARTESIAN_POINT ( 'NONE',  ( -1.767766952966369098, 1.767766952966369098, -2.299999997815050712 ) ) ;
#13283 = CARTESIAN_POINT ( 'NONE',  ( 0.000000000000000000, 184.0000000000000000, 7.000000000000000000 ) ) ;
#13284 = DIRECTION ( 'NONE',  ( -3.326610055774640964E-18, 1.000000000000000000, 2.775557561562888393E-16 ) ) ;
#13285 = CARTESIAN_POINT ( 'NONE',  ( 1.767766952966368654, 1.767766952966369098, 0.6000000000000000888 ) ) ;
#13286 = CARTESIAN_POINT ( 'NONE',  ( 5.486982057989152395, 2.429327048029968683, 4.200681937418260681 ) ) ;
#13287 = CARTESIAN_POINT ( 'NONE',  ( 5.317509234263963158, 2.779225709350988449, 11.63236078583908650 ) ) ;
#13288 = EDGE_CURVE ( 'NONE', #5259, #320, #9070, .T. ) ;
#13289 = ORIENTED_EDGE ( 'NONE', *, *, #2065, .F. ) ;
#13290 = CIRCLE ( 'NONE', #11256, 6.000000000000000000 ) ;
#13291 = EDGE_CURVE ( 'NONE', #12484, #920, #13162, .T. ) ;
#13292 = EDGE_LOOP ( 'NONE', ( #2714, #876, #1582, #2068 ) ) ;
#13293 = VERTEX_POINT ( 'NONE', #3403 ) ;
#13294 = CARTESIAN_POINT ( 'NONE',  ( -2.692215568229873401, 5.362327947133580075, 11.76229037835932978 ) ) ;
#13295 = ORIENTED_EDGE ( 'NONE', *, *, #10002, .T. ) ;
#13296 = CARTESIAN_POINT ( 'NONE',  ( -2.500000000000000444, 1.035533905932737753, -2.249999997815050445 ) ) ;
#13297 = CARTESIAN_POINT ( 'NONE',  ( -9.750000000000003553, 19.99999999999999645, -1.500000000000033751 ) ) ;
#13298 = CARTESIAN_POINT ( 'NONE',  ( 6.172614129015227213, 0.9817721000789304542, 31.26236973443873879 ) ) ;
#13299 = CARTESIAN_POINT ( 'NONE',  ( -0.8561741729129469514, 187.3999999989075889, 9.066987299999999195 ) ) ;
#13300 = AXIS2_PLACEMENT_3D ( 'NONE', #9876, #6063, #10982 ) ;
#13301 = CARTESIAN_POINT ( 'NONE',  ( -2.500000000000000000, 0.000000000000000000, 0.9000000000000000222 ) ) ;
#13302 = CARTESIAN_POINT ( 'NONE',  ( -5.330004929009606762, 2.755647751839361170, 31.26239891805596827 ) ) ;
#13303 = CARTESIAN_POINT ( 'NONE',  ( 0.8561741729129463963, -2.066987299999999195, -1.699999998907525400 ) ) ;
#13304 = CARTESIAN_POINT ( 'NONE',  ( 4.416779112813693509, -4.422345839825757352, 30.73774718278283302 ) ) ;
#13305 = CARTESIAN_POINT ( 'NONE',  ( -2.974673115704016713, 227.4156934420934419, 7.698994310615434600 ) ) ;
#13306 = CARTESIAN_POINT ( 'NONE',  ( -12.50000000000000533, 0.000000000000000000, 0.000000000000000000 ) ) ;
#13307 = EDGE_LOOP ( 'NONE', ( #3100, #11040, #11540, #10261, #7658, #4134 ) ) ;
#13308 = ORIENTED_EDGE ( 'NONE', *, *, #8079, .F. ) ;
#13309 = ORIENTED_EDGE ( 'NONE', *, *, #8379, .F. ) ;
#13310 = ORIENTED_EDGE ( 'NONE', *, *, #13510, .F. ) ;
#13311 = CARTESIAN_POINT ( 'NONE',  ( -5.558508435838135142, 2.857531096719037489, 24.49999999999999289 ) ) ;
#13312 = CARTESIAN_POINT ( 'NONE',  ( 0.000000000000000000, 19.99999999999999645, 12.50000000000000355 ) ) ;
#13313 = CARTESIAN_POINT ( 'NONE',  ( -2.500000000000000444, 185.2000000000000171, 7.000000000000000000 ) ) ;
#13314 = DIRECTION ( 'NONE',  ( -0.000000000000000000, -1.000000000000000000, -0.000000000000000000 ) ) ;
#13315 = UNCERTAINTY_MEASURE_WITH_UNIT (LENGTH_MEASURE( 1.000000000000000082E-05 ), #7998, 'distance_accuracy_value', 'NONE');
#13316 = CARTESIAN_POINT ( 'NONE',  ( 6.780834062235653815E-14, 6.000000000000000888, 10.49999999999998224 ) ) ;
#13317 = CARTESIAN_POINT ( 'NONE',  ( -3.420311045507815617, -4.931422832349310781, 12.50007961174474502 ) ) ;
#13318 = CARTESIAN_POINT ( 'NONE',  ( 0.000000000000000000, 0.000000000000000000, 52.97056274847714263 ) ) ;
#13319 = CARTESIAN_POINT ( 'NONE',  ( 0.1323933160976972501, -6.000000000000000000, 18.99999999999998934 ) ) ;
#13320 = PLANE ( 'NONE',  #10747 ) ;
#13321 = DIRECTION ( 'NONE',  ( 0.000000000000000000, -1.000000000000000000, 0.000000000000000000 ) ) ;
#13322 = CARTESIAN_POINT ( 'NONE',  ( 2.500000000000000444, 188.7499999978150527, 5.964466094067262247 ) ) ;
#13323 = CARTESIAN_POINT ( 'NONE',  ( 2.050915569729614862, 227.9948459642048419, 9.402920486592190485 ) ) ;
#13324 = CARTESIAN_POINT ( 'NONE',  ( 5.317509234263963158, 2.779225709350988449, 11.49999999999998224 ) ) ;
#13325 =( BOUNDED_CURVE ( )  B_SPLINE_CURVE ( 2, ( #5923, #10769, #10843, #15470, #15706, #7276, #12112, #9340, #14181 ),
 .UNSPECIFIED., .F., .F. ) 
 B_SPLINE_CURVE_WITH_KNOTS ( ( 3, 2, 2, 2, 3 ),
 ( 0.6428571428571429047, 0.6607142857142856984, 0.6785714285714286031, 0.6964285714285713969, 0.7142857142857143016 ),
 .UNSPECIFIED. ) 
 CURVE ( )  GEOMETRIC_REPRESENTATION_ITEM ( )  RATIONAL_B_SPLINE_CURVE ( ( 1.000000000000000000, 0.9238795325112867385, 1.000000000000000000, 0.9238795325112867385, 1.000000000000000000, 0.9238795325112867385, 1.000000000000000000, 0.9238795325112867385, 1.000000000000000000 ) ) 
 REPRESENTATION_ITEM ( '' )  );
#13326 = CARTESIAN_POINT ( 'NONE',  ( -2.375777824384393888, 189.9842224717010879, 5.389868150937594748 ) ) ;
#13327 = EDGE_CURVE ( 'NONE', #10284, #9576, #10118, .T. ) ;
#13328 = VERTEX_POINT ( 'NONE', #7950 ) ;
#13329 = FACE_OUTER_BOUND ( 'NONE', #10017, .T. ) ;
#13330 = CARTESIAN_POINT ( 'NONE',  ( 0.6139908388541727158, -5.969238533166604022, 10.69977627912011187 ) ) ;
#13332 = ORIENTED_EDGE ( 'NONE', *, *, #2651, .F. ) ;
#13331 = CARTESIAN_POINT ( 'NONE',  ( 5.317509234264027107, 2.779225709350867213, 24.63236078583910071 ) ) ;
#13333 = CARTESIAN_POINT ( 'NONE',  ( 2.817313151351127587, -5.579000502529462224, 11.49999999999998224 ) ) ;
#13334 = CARTESIAN_POINT ( 'NONE',  ( -5.385276659965230388E-16, 226.3251816629291966, 4.486670979098442480 ) ) ;
#13335 = CARTESIAN_POINT ( 'NONE',  ( 3.566234721237914407, 5.134387337253918382, 23.50008258189710375 ) ) ;
#13336 =( BOUNDED_CURVE ( )  B_SPLINE_CURVE ( 2, ( #2878, #1905, #13768, #7963, #10350, #6548, #10122, #9166, #12803 ),
 .UNSPECIFIED., .F., .F. ) 
 B_SPLINE_CURVE_WITH_KNOTS ( ( 3, 2, 2, 2, 3 ),
 ( 0.6428571428571429047, 0.6607142857142856984, 0.6785714285714286031, 0.6964285714285713969, 0.7142857142857143016 ),
 .UNSPECIFIED. ) 
 CURVE ( )  GEOMETRIC_REPRESENTATION_ITEM ( )  RATIONAL_B_SPLINE_CURVE ( ( 1.000000000000000000, 0.9238795325112867385, 1.000000000000000000, 0.9238795325112867385, 1.000000000000000000, 0.9238795325112867385, 1.000000000000000000, 0.9238795325112867385, 1.000000000000000000 ) ) 
 REPRESENTATION_ITEM ( '' )  );
#13337 = AXIS2_PLACEMENT_3D ( 'NONE', #6246, #7660, #9899 ) ;
#13338 = CARTESIAN_POINT ( 'NONE',  ( -1.265664690411614835E-16, 2.066987299999999639, 2.050000001092474822 ) ) ;
#13339 = FACE_OUTER_BOUND ( 'NONE', #11164, .T. ) ;
#13340 = CARTESIAN_POINT ( 'NONE',  ( -0.5030929395820097350, -6.230885867001147993, 30.12600319116549485 ) ) ;
#13341 = CARTESIAN_POINT ( 'NONE',  ( -2.500000000000000888, 188.3800000002185016, 8.035533905932737753 ) ) ;
#13342 = CARTESIAN_POINT ( 'NONE',  ( -1.223735324759350984, 228.7813039559728168, 8.495841244274044968 ) ) ;
#13343 = CARTESIAN_POINT ( 'NONE',  ( 1.691241850060078322, 228.6046986201012601, 7.985794961368397615 ) ) ;
#13344 = CARTESIAN_POINT ( 'NONE',  ( 3.796994071234844259E-16, -2.066987299999999639, 1.650000001092474911 ) ) ;
#13345 = CARTESIAN_POINT ( 'NONE',  ( 5.649053410273092268, 2.675685104943213766, 17.38482219624156855 ) ) ;
#13346 = ORIENTED_EDGE ( 'NONE', *, *, #3894, .F. ) ;
#13347 = CARTESIAN_POINT ( 'NONE',  ( 2.066987300000000971, 186.6999999989075150, 6.143825827087054492 ) ) ;
#13348 = CARTESIAN_POINT ( 'NONE',  ( -0.8561741729129457301, 185.2999999989075377, 4.933012699999999029 ) ) ;
#13349 = DIRECTION ( 'NONE',  ( 0.5877852522924802425, -0.8090169943749422332, 0.000000000000000000 ) ) ;
#13350 = VECTOR ( 'NONE', #10555, 1000.000000000000114 ) ;
#13351 = VECTOR ( 'NONE', #11476, 1000.000000000000000 ) ;
#13352 = EDGE_LOOP ( 'NONE', ( #5200, #6030 ) ) ;
#13353 = CARTESIAN_POINT ( 'NONE',  ( -3.000000000000000000, 0.000000000000000000, 5.000000000000004441 ) ) ;
#13354 = LINE ( 'NONE', #12162, #2640 ) ;
#13355 = FACE_OUTER_BOUND ( 'NONE', #14547, .T. ) ;
#13356 = CARTESIAN_POINT ( 'NONE',  ( 0.8561741729129455081, 189.1999999989075434, 4.933012699999999029 ) ) ;
#13357 = CARTESIAN_POINT ( 'NONE',  ( 4.142173849413805620, -4.341773579105349334, 30.38480617551148910 ) ) ;
#13358 = CARTESIAN_POINT ( 'NONE',  ( -1.035533905932737753, 2.500000000000000444, -2.349999997815050090 ) ) ;
#13359 = FACE_OUTER_BOUND ( 'NONE', #5340, .T. ) ;
#13360 = CARTESIAN_POINT ( 'NONE',  ( -5.935543223013850955, 0.8771126767607324570, 11.49999999999998224 ) ) ;
#13361 = CARTESIAN_POINT ( 'NONE',  ( -2.997753866155832725, 5.484939622623836719, 30.38439807107077684 ) ) ;
#13362 = CARTESIAN_POINT ( 'NONE',  ( 9.750000000000003553, 184.0000000000000000, 1.500000000000101696 ) ) ;
#13363 = CARTESIAN_POINT ( 'NONE',  ( 1.035533905932737753, 187.3499999999999943, 4.500000000000001776 ) ) ;
#13364 = VERTEX_POINT ( 'NONE', #15271 ) ;
#13365 = ORIENTED_EDGE ( 'NONE', *, *, #14189, .F. ) ;
#13366 = ORIENTED_EDGE ( 'NONE', *, *, #1640, .T. ) ;
#13367 = CARTESIAN_POINT ( 'NONE',  ( -5.487348639458788035, -2.428538342494640290, 25.30022217383879024 ) ) ;
#13368 = ORIENTED_EDGE ( 'NONE', *, *, #6135, .F. ) ;
#13369 = CARTESIAN_POINT ( 'NONE',  ( 1.767766952966369320, -1.767766952966368654, -2.699999997815051067 ) ) ;
#13370 = CARTESIAN_POINT ( 'NONE',  ( 0.000000000000000000, 184.0000000000000000, 7.000000000000000000 ) ) ;
#13371 = DIRECTION ( 'NONE',  ( -0.000000000000000000, -1.000000000000000000, -0.000000000000000000 ) ) ;
#13372 = CARTESIAN_POINT ( 'NONE',  ( -6.403569081242510563E-16, 188.2499999989075263, 9.066987300000000971 ) ) ;
#13373 = CARTESIAN_POINT ( 'NONE',  ( -1.767766952966369098, 1.767766952966369098, 2.400000000000000355 ) ) ;
#13374 = EDGE_CURVE ( 'NONE', #15059, #471, #15593, .T. ) ;
#13375 = DIRECTION ( 'NONE',  ( 0.000000000000000000, 0.000000000000000000, 1.000000000000000000 ) ) ;
#13376 = CARTESIAN_POINT ( 'NONE',  ( -5.859221468178898107, -2.178708437343367166, 25.47408542334170534 ) ) ;
#13377 = CARTESIAN_POINT ( 'NONE',  ( -0.8561741729129458411, -2.066987299999999195, 1.600000001092474866 ) ) ;
#13378 = CARTESIAN_POINT ( 'NONE',  ( -3.827021247335478803E-16, 2.500000000000000000, -2.500000000000000000 ) ) ;
#13379 = CARTESIAN_POINT ( 'NONE',  ( -2.692660167145737304, 226.8630334657495666, 6.071693271619351684 ) ) ;
#13380 = AXIS2_PLACEMENT_3D ( 'NONE', #1563, #11116, #3792 ) ;
#13381 = CARTESIAN_POINT ( 'NONE',  ( 2.999999999999999556, 1.732050807568877859, -5.500000000000000000 ) ) ;
#13382 = ORIENTED_EDGE ( 'NONE', *, *, #6976, .F. ) ;
#13383 = ORIENTED_EDGE ( 'NONE', *, *, #445, .F. ) ;
#13384 = ORIENTED_EDGE ( 'NONE', *, *, #12599, .F. ) ;
#13385 = ORIENTED_EDGE ( 'NONE', *, *, #12732, .F. ) ;
#13386 = CARTESIAN_POINT ( 'NONE',  ( -5.769755079862290081, -2.405651898699045610, 30.12694108445699825 ) ) ;
#13387 = ADVANCED_FACE ( 'NONE', ( #14468 ), #14711, .F. ) ;
#13388 = FACE_OUTER_BOUND ( 'NONE', #8929, .T. ) ;
#13389 = CYLINDRICAL_SURFACE ( 'NONE', #12165, 2.000000000000000000 ) ;
#13390 = CARTESIAN_POINT ( 'NONE',  ( -5.648794263291781803, 2.676232015153535926, 31.61441947245485196 ) ) ;
#13391 = AXIS2_PLACEMENT_3D ( 'NONE', #12540, #6357, #11193 ) ;
#13392 = EDGE_CURVE ( 'NONE', #9005, #1272, #8951, .T. ) ;
#13393 = CARTESIAN_POINT ( 'NONE',  ( 4.344313232727033736, -4.493553492990184139, 23.99563030319847456 ) ) ;
#13394 = CARTESIAN_POINT ( 'NONE',  ( 2.030576276931546336E-13, -6.250000000000000888, 25.49999999999999645 ) ) ;
#13395 = CARTESIAN_POINT ( 'NONE',  ( -9.750000000000003553, 3.401296724241641415E-14, 0.000000000000000000 ) ) ;
#13396 = B_SPLINE_CURVE_WITH_KNOTS ( 'NONE', 1,
 ( #14209, #3319 ),
 .UNSPECIFIED., .F., .F.,
 ( 2, 2 ),
 ( 0.000000000000000000, 1.000000000000000000 ),
 .UNSPECIFIED. ) ;
#13397 = CARTESIAN_POINT ( 'NONE',  ( -5.615811513734916716, -2.743665920700641525, 23.99691356133952524 ) ) ;
#13398 = DIRECTION ( 'NONE',  ( -0.9996329569789847991, -0.0003848699982329016438, -0.02708880205058770627 ) ) ;
#13399 = DIRECTION ( 'NONE',  ( 6.982962677686266711E-15, 0.000000000000000000, -1.000000000000000000 ) ) ;
#13400 = PRODUCT_DEFINITION_SHAPE ( 'NONE', 'NONE',  #15758 ) ;
#13401 = CARTESIAN_POINT ( 'NONE',  ( 1.035533905932738197, 187.7499999978150527, 9.500000000000003553 ) ) ;
#13402 = CARTESIAN_POINT ( 'NONE',  ( 2.600554376340839635, 226.8075635770346139, 5.908288162427849599 ) ) ;
#13403 = DIRECTION ( 'NONE',  ( -0.000000000000000000, 1.000000000000000000, -0.000000000000000000 ) ) ;
#13404 = CARTESIAN_POINT ( 'NONE',  ( 5.931828553037968632, 0.9033193133619482618, 11.23805675996852571 ) ) ;
#13405 = VECTOR ( 'NONE', #3181, 1000.000000000000000 ) ;
#13406 = CARTESIAN_POINT ( 'NONE',  ( -2.990007448523356537, 189.8992274272603993, 6.832429650438955449 ) ) ;
#13407 = ADVANCED_FACE ( 'NONE', ( #13193 ), #8437, .T. ) ;
#13408 = VERTEX_POINT ( 'NONE', #14631 ) ;
#13409 = CARTESIAN_POINT ( 'NONE',  ( -5.665308849928823776, 1.980336949702511173, 12.49992002356259668 ) ) ;
#13410 = CARTESIAN_POINT ( 'NONE',  ( 0.1323933160976290824, -6.000000000000000000, 12.49999999999998579 ) ) ;
#13411 = CARTESIAN_POINT ( 'NONE',  ( 5.531757352715640508, 2.326874507723235563, 25.37380682714710645 ) ) ;
#13412 = CARTESIAN_POINT ( 'NONE',  ( 4.435347140101058905, -4.403429997944485308, 31.13234125634170368 ) ) ;
#13413 = CARTESIAN_POINT ( 'NONE',  ( 1.104763767215224401, 226.3928744374965447, 4.686231709593007722 ) ) ;
#13414 = AXIS2_PLACEMENT_3D ( 'NONE', #13834, #5104, #2946 ) ;
#13415 = CARTESIAN_POINT ( 'NONE',  ( 1.353717517954364224E-13, -6.250000000000000888, 18.99999999999998934 ) ) ;
#13416 = AXIS2_PLACEMENT_3D ( 'NONE', #230, #72, #1261 ) ;
#13417 = CARTESIAN_POINT ( 'NONE',  ( -0.8561741729129458411, -2.066987299999999195, 0.8000000010924747107 ) ) ;
#13418 = CARTESIAN_POINT ( 'NONE',  ( -4.435347140101218777, 4.403429997944323659, 24.49999999999999289 ) ) ;
#13419 = SURFACE_STYLE_USAGE ( .BOTH. , #215 ) ;
#13420 = EDGE_CURVE ( 'NONE', #3400, #11314, #4853, .T. ) ;
#13421 = CARTESIAN_POINT ( 'NONE',  ( -6.105861027178951517, 1.337741388556971778, 12.29954462468842458 ) ) ;
#13422 =( BOUNDED_CURVE ( )  B_SPLINE_CURVE ( 2, ( #9451, #8021, #10489, #10640, #776, #15343, #15418, #4517, #14368 ),
 .UNSPECIFIED., .F., .F. ) 
 B_SPLINE_CURVE_WITH_KNOTS ( ( 3, 2, 2, 2, 3 ),
 ( 0.3571428571428571508, 0.3750000000000000000, 0.3928571428571428492, 0.4107142857142856984, 0.4285714285714285476 ),
 .UNSPECIFIED. ) 
 CURVE ( )  GEOMETRIC_REPRESENTATION_ITEM ( )  RATIONAL_B_SPLINE_CURVE ( ( 1.000000000000000000, 0.9238795325112867385, 1.000000000000000000, 0.9238795325112867385, 1.000000000000000000, 0.9238795325112867385, 1.000000000000000000, 0.9238795325112867385, 1.000000000000000000 ) ) 
 REPRESENTATION_ITEM ( '' )  );
#13423 = CARTESIAN_POINT ( 'NONE',  ( -2.500000000000000444, 184.3499999999999943, 5.964466094067261359 ) ) ;
#13424 = FACE_BOUND ( 'NONE', #9856, .T. ) ;
#13425 = CARTESIAN_POINT ( 'NONE',  ( 0.3231974900581740529, 228.9035839249116009, 8.848992768962338218 ) ) ;
#13426 = CARTESIAN_POINT ( 'NONE',  ( 0.8561741729129452860, 2.066987299999999639, 0.4000000010924748550 ) ) ;
#13427 = CARTESIAN_POINT ( 'NONE',  ( 5.570760634536900291, -2.834026536768054605, 24.76225281721715987 ) ) ;
#13428 = ADVANCED_FACE ( 'NONE', ( #2209 ), #10732, .F. ) ;
#13429 = VERTEX_POINT ( 'NONE', #13273 ) ;
#13430 = CARTESIAN_POINT ( 'NONE',  ( -9.825582188149883933E-17, 187.6499999989075320, 4.933012699999999029 ) ) ;
#13431 = AXIS2_PLACEMENT_3D ( 'NONE', #5943, #4829, #10788 ) ;
#13432 = CARTESIAN_POINT ( 'NONE',  ( -9.825582188149883933E-17, 187.6499999989075320, 4.933012699999999029 ) ) ;
#13433 = DIRECTION ( 'NONE',  ( -1.000000000000000000, -6.123233995736782060E-17, 0.000000000000000000 ) ) ;
#13435 = VERTEX_POINT ( 'NONE', #3721 ) ;
#13434 = CARTESIAN_POINT ( 'NONE',  ( 4.286401442266448925, -4.198423832313278758, 24.63236078583909716 ) ) ;
#13436 = DIRECTION ( 'NONE',  ( -1.000000000000000000, 0.000000000000000000, 0.000000000000000000 ) ) ;
#13437 = CARTESIAN_POINT ( 'NONE',  ( -9.148167235839370302E-31, 182.0000000000000000, 4.500000000000000888 ) ) ;
#13438 = CARTESIAN_POINT ( 'NONE',  ( 0.000000000000000000, 22.00000000000000000, 12.50000000000000355 ) ) ;
#13439 = CARTESIAN_POINT ( 'NONE',  ( 5.999999999999999112, 201.6409668649147022, 13.30942870683726120 ) ) ;
#13440 = CARTESIAN_POINT ( 'NONE',  ( -1.965116437629976787E-16, 189.2499999989075263, 4.933012699999999029 ) ) ;
#13441 = AXIS2_PLACEMENT_3D ( 'NONE', #2987, #5615, #827 ) ;
#13442 = DIRECTION ( 'NONE',  ( 1.000000000000000000, 0.000000000000000000, 0.000000000000000000 ) ) ;
#13443 = CARTESIAN_POINT ( 'NONE',  ( 2.500000000000000000, 3.061616997868383141E-16, -2.599999997815050534 ) ) ;
#13444 = CYLINDRICAL_SURFACE ( 'NONE', #956, 2.500000000000000444 ) ;
#13445 = CARTESIAN_POINT ( 'NONE',  ( 5.915755444410815578, -1.003187219519776852, 10.99687951097621408 ) ) ;
#13446 = CARTESIAN_POINT ( 'NONE',  ( -5.317509234263939177, 2.779225709351034634, 11.36935038651144758 ) ) ;
#13447 = CARTESIAN_POINT ( 'NONE',  ( -2.066760391300492827E-16, 189.4499999989075150, 4.933012699999999029 ) ) ;
#13448 = CARTESIAN_POINT ( 'NONE',  ( 2.668367453516444776, 5.373994336898222812, 24.49999999999999289 ) ) ;
#13449 = VERTEX_POINT ( 'NONE', #1102 ) ;
#13450 = ORIENTED_EDGE ( 'NONE', *, *, #11539, .T. ) ;
#13451 = MECHANICAL_DESIGN_GEOMETRIC_PRESENTATION_REPRESENTATION (  '', ( #12427 ), #6853 ) ;
#13452 = ORIENTED_EDGE ( 'NONE', *, *, #3504, .F. ) ;
#13453 = FACE_OUTER_BOUND ( 'NONE', #14507, .T. ) ;
#13454 = EDGE_LOOP ( 'NONE', ( #9121, #4311, #6067, #8946 ) ) ;
#13455 = CARTESIAN_POINT ( 'NONE',  ( -1.461580736456472351, -1.461580736456473018, -1.049999998907525489 ) ) ;
#13456 = CARTESIAN_POINT ( 'NONE',  ( -5.648559266344491903, -2.676764518776009627, 12.11396179408069784 ) ) ;
#13457 = CARTESIAN_POINT ( 'NONE',  ( -25.39999999999994884, 0.000000000000000000, 0.000000000000000000 ) ) ;
#13458 = CARTESIAN_POINT ( 'NONE',  ( 1.461580736456472795, 186.9499999989075150, 5.538419263543527649 ) ) ;
#13459 = CARTESIAN_POINT ( 'NONE',  ( 1.035533905932739085, -2.500000000000000000, 0.3500000000000000333 ) ) ;
#13460 = CARTESIAN_POINT ( 'NONE',  ( 0.8499999999999896527, 0.000000000000000000, 0.000000000000000000 ) ) ;
#13461 = ITEM_DEFINED_TRANSFORMATION ( 'NONE', 'NONE', #8139,  #14201 ) ;
#13462 = CARTESIAN_POINT ( 'NONE',  ( 4.005998022989971652, 4.467726698309252065, 5.799318062581741984 ) ) ;
#13463 = CARTESIAN_POINT ( 'NONE',  ( 1.461580736456473018, -1.461580736456472573, -0.8499999989075254225 ) ) ;
#13464 = CARTESIAN_POINT ( 'NONE',  ( -5.903843691985246167, 2.055287728870609509, 29.99995093123466816 ) ) ;
#13465 = CARTESIAN_POINT ( 'NONE',  ( -2.439580969806472321, 226.7272467340407331, 5.671663139905907869 ) ) ;
#13466 = VERTEX_POINT ( 'NONE', #2371 ) ;
#13467 = VERTEX_POINT ( 'NONE', #7078 ) ;
#13468 = ORIENTED_EDGE ( 'NONE', *, *, #3370, .T. ) ;
#13469 = CARTESIAN_POINT ( 'NONE',  ( -5.725684683139582454, -2.507514573674833880, 10.70112161576659915 ) ) ;
#13470 = EDGE_CURVE ( 'NONE', #6637, #3564, #15194, .T. ) ;
#13471 = CARTESIAN_POINT ( 'NONE',  ( 2.817313151351108047, 5.579000502529472882, 5.000000000000004441 ) ) ;
#13472 = CARTESIAN_POINT ( 'NONE',  ( 0.1323408341374891217, 6.250000000000000888, 6.000000000000006217 ) ) ;
#13473 = CARTESIAN_POINT ( 'NONE',  ( -5.903061651806624788, 2.057626436184726515, 31.99991741810289625 ) ) ;
#13474 = CARTESIAN_POINT ( 'NONE',  ( 0.8730424326981676142, 5.936362132114451740, 10.99500690218562937 ) ) ;
#13475 = FACE_OUTER_BOUND ( 'NONE', #14569, .T. ) ;
#13476 = CARTESIAN_POINT ( 'NONE',  ( 5.329945432499647140, -2.755769831645103363, 11.76229037835932800 ) ) ;
#13477 = CARTESIAN_POINT ( 'NONE',  ( -6.142908455506942644, -1.155755562476059817, 5.615177803758428787 ) ) ;
#13478 = DIRECTION ( 'NONE',  ( 0.000000000000000000, 0.000000000000000000, -1.000000000000000000 ) ) ;
#13479 = DIRECTION ( 'NONE',  ( 0.000000000000000000, -1.000000000000000000, 0.000000000000000000 ) ) ;
#13480 = CARTESIAN_POINT ( 'NONE',  ( -1.035533905932737975, 187.3499999978151038, 4.500000000000000888 ) ) ;
#13481 = CARTESIAN_POINT ( 'NONE',  ( 3.000032282732917555, 227.2742683068891552, 7.282695486718367306 ) ) ;
#13482 = EDGE_CURVE ( 'NONE', #6460, #3929, #14635, .T. ) ;
#13483 = CARTESIAN_POINT ( 'NONE',  ( -0.4481745786268478415, 189.0473500653932319, 10.15604835757928726 ) ) ;
#13484 = VERTEX_POINT ( 'NONE', #9628 ) ;
#13485 = EDGE_CURVE ( 'NONE', #1423, #13328, #2850, .T. ) ;
#13486 = CARTESIAN_POINT ( 'NONE',  ( -2.668367453516709009, 5.373994336898094026, 5.132393880016356214 ) ) ;
#13487 = DIRECTION ( 'NONE',  ( -0.000000000000000000, 1.000000000000000000, -0.000000000000000000 ) ) ;
#13488 = CARTESIAN_POINT ( 'NONE',  ( -1.767766952966369098, 1.767766952966369098, -0.7999999999999999334 ) ) ;
#13489 = CARTESIAN_POINT ( 'NONE',  ( 3.780072143464270784, -4.979057943639705996, 32.00008219321556169 ) ) ;
#13490 = CARTESIAN_POINT ( 'NONE',  ( 2.057832045933806420, 226.5876095930653094, 5.260198610313286061 ) ) ;
#13491 = CARTESIAN_POINT ( 'NONE',  ( 3.458623254138554870, 5.207221900902925249, 23.52622717124731011 ) ) ;
#13492 = CARTESIAN_POINT ( 'NONE',  ( 2.066987299999999639, 2.531329380823229670E-16, -0.5499999989075250451 ) ) ;
#13493 = CARTESIAN_POINT ( 'NONE',  ( 5.487097279078438916, -2.429065649168797858, 4.200479458972859348 ) ) ;
#13494 = CARTESIAN_POINT ( 'NONE',  ( -5.558508435838198203, 2.857531096718914476, 11.49999999999998224 ) ) ;
#13495 = CARTESIAN_POINT ( 'NONE',  ( -2.500000000000000444, 184.4499999999999886, 8.035533905932737753 ) ) ;
#13496 = DIRECTION ( 'NONE',  ( -1.000000000000000000, 0.000000000000000000, 0.000000000000000000 ) ) ;
#13497 = CARTESIAN_POINT ( 'NONE',  ( 1.990705347729657237, 228.2501094229765215, 6.961721135629644230 ) ) ;
#13498 = CARTESIAN_POINT ( 'NONE',  ( 0.000000000000000000, 184.0000000000000000, 7.000000000000000000 ) ) ;
#13499 = CARTESIAN_POINT ( 'NONE',  ( 6.768587589771821120E-14, -6.000000000000000888, 12.49999999999998401 ) ) ;
#13500 = ORIENTED_EDGE ( 'NONE', *, *, #6980, .F. ) ;
#13502 = DIRECTION ( 'NONE',  ( -0.000000000000000000, 1.000000000000000000, -0.000000000000000000 ) ) ;
#13501 = PRODUCT_DEFINITION_SHAPE ( 'NONE', 'NONE',  #13615 ) ;
#13503 = CARTESIAN_POINT ( 'NONE',  ( -1.461580736456473240, 186.9499999989075150, 5.538419263543526760 ) ) ;
#13504 = CARTESIAN_POINT ( 'NONE',  ( -5.666074146197956907, -1.978051345703274011, 19.00004932073311181 ) ) ;
#13506 = ORIENTED_EDGE ( 'NONE', *, *, #15100, .F. ) ;
#13505 = CARTESIAN_POINT ( 'NONE',  ( 4.153440676704409640, 4.671190581744483872, 30.20045537531156654 ) ) ;
#13507 = LINE ( 'NONE', #228, #15181 ) ;
#13508 = CARTESIAN_POINT ( 'NONE',  ( 5.570760634536812361, -2.834026536768229576, 31.26225281721713145 ) ) ;
#13509 = CARTESIAN_POINT ( 'NONE',  ( 0.2637975869347859437, 6.245592211692893692, 12.47332839949191197 ) ) ;
#13510 = EDGE_CURVE ( 'NONE', #1465, #6001, #4774, .T. ) ;
#13511 = CARTESIAN_POINT ( 'NONE',  ( -0.8983937855600439004, 189.0000000000000284, 9.343143558360589296 ) ) ;
#13512 = CARTESIAN_POINT ( 'NONE',  ( 0.000000000000000000, 0.000000000000000000, 2.000000000000001776 ) ) ;
#13513 = VECTOR ( 'NONE', #7450, 1000.000000000000114 ) ;
#13514 = CARTESIAN_POINT ( 'NONE',  ( 5.558508435838221295, 2.857531096718871844, 11.49999999999998224 ) ) ;
#13515 = DIRECTION ( 'NONE',  ( 0.000000000000000000, -1.000000000000000000, 0.000000000000000000 ) ) ;
#13516 = CARTESIAN_POINT ( 'NONE',  ( -1.084202172485504434E-15, -3.464101615137755275, -5.500000000000000000 ) ) ;
#13517 = CARTESIAN_POINT ( 'NONE',  ( 1.353717517954364224E-13, -6.250000000000000888, 18.99999999999998934 ) ) ;
#13518 = EDGE_CURVE ( 'NONE', #5609, #2306, #3802, .T. ) ;
#13519 = CARTESIAN_POINT ( 'NONE',  ( 3.735808404764840329, 4.696639218303251262, 23.52601979877760030 ) ) ;
#13520 = ORIENTED_EDGE ( 'NONE', *, *, #7856, .T. ) ;
#13521 = CARTESIAN_POINT ( 'NONE',  ( 0.8561741729129455081, 186.9999999989074979, 4.933012699999999029 ) ) ;
#13522 = ORIENTED_EDGE ( 'NONE', *, *, #10127, .T. ) ;
#13523 = ORIENTED_EDGE ( 'NONE', *, *, #4466, .T. ) ;
#13524 = EDGE_CURVE ( 'NONE', #15573, #2516, #6102, .T. ) ;
#13525 = AXIS2_PLACEMENT_3D ( 'NONE', #10408, #15340, #14971 ) ;
#13526 = B_SPLINE_CURVE_WITH_KNOTS ( 'NONE', 3,
 ( #10956, #4921, #1091, #13340, #216, #14778, #2525, #3864, #7454, #10881, #13262, #9615, #2443, #2280, #8425, #4842, #3711, #1246 ),
 .UNSPECIFIED., .F., .F.,
 ( 4, 2, 2, 2, 2, 2, 2, 2, 4 ),
 ( 0.003131490185286079676, 0.003522829482338674534, 0.003914168779391269393, 0.004305508076443864685, 0.004696847373496459976, 0.005088186670549064809, 0.005479525967601669642, 0.005870865264654275342, 0.006262204561706881042 ),
 .UNSPECIFIED. ) ;
#13527 = CARTESIAN_POINT ( 'NONE',  ( 2.500000000000000000, 3.061616997868383141E-16, 2.500000000000000000 ) ) ;
#13528 = VERTEX_POINT ( 'NONE', #12386 ) ;
#13529 = CARTESIAN_POINT ( 'NONE',  ( 0.8561741729129451750, 2.066987299999999639, 0.2000000010924747329 ) ) ;
#13530 = CARTESIAN_POINT ( 'NONE',  ( -6.021167129161037579, -1.680051667990365871, 12.47359571723300142 ) ) ;
#13531 = FACE_OUTER_BOUND ( 'NONE', #10871, .T. ) ;
#13532 = FACE_OUTER_BOUND ( 'NONE', #14006, .T. ) ;
#13533 = CARTESIAN_POINT ( 'NONE',  ( 2.500000000000000444, -1.035533905932737309, 1.250000000000000222 ) ) ;
#13534 = DIRECTION ( 'NONE',  ( 1.000000000000000000, 0.000000000000000000, 0.000000000000000000 ) ) ;
#13535 = CONTEXT_DEPENDENT_SHAPE_REPRESENTATION ( #4054, #3348 ) ;
#13536 = CARTESIAN_POINT ( 'NONE',  ( 0.000000000000000000, 0.000000000000000000, 36.00000000000000711 ) ) ;
#13537 = CARTESIAN_POINT ( 'NONE',  ( -0.8561741729129455081, 2.066987299999999639, -2.899999998907526244 ) ) ;
#13538 = AXIS2_PLACEMENT_3D ( 'NONE', #7189, #254, #14741 ) ;
#13539 = CARTESIAN_POINT ( 'NONE',  ( -6.105925084677703119, 1.337450587213082631, 30.20066851092422411 ) ) ;
#13540 = CARTESIAN_POINT ( 'NONE',  ( -1.329004440443209090, 226.4243434115648199, 4.778997713384572243 ) ) ;
#13541 = VERTEX_POINT ( 'NONE', #12309 ) ;
#13542 = ORIENTED_EDGE ( 'NONE', *, *, #10850, .T. ) ;
#13543 = ORIENTED_EDGE ( 'NONE', *, *, #158, .T. ) ;
#13544 = CARTESIAN_POINT ( 'NONE',  ( 0.1306171417089971032, 5.999999999999999112, 16.99999999999998224 ) ) ;
#13545 = CARTESIAN_POINT ( 'NONE',  ( -3.118365096457675456, 189.0000000000000000, -7.000000000000000000 ) ) ;
#13546 = CARTESIAN_POINT ( 'NONE',  ( 0.6156133477426871670, 6.220296490279942248, 5.798723873455116973 ) ) ;
#13547 = CARTESIAN_POINT ( 'NONE',  ( 0.9999505860954734926, -6.169489349035784720, 18.13105903165811839 ) ) ;
#13548 = CARTESIAN_POINT ( 'NONE',  ( 6.768587589771821120E-14, 6.000000000000000888, 12.49999999999998401 ) ) ;
#13549 = CARTESIAN_POINT ( 'NONE',  ( -2.500000000000000444, 187.4499999978150981, 5.964466094067261359 ) ) ;
#13550 = CARTESIAN_POINT ( 'NONE',  ( 2.066987300000000083, 184.9999999989074979, 7.856174172912946396 ) ) ;
#13551 = CARTESIAN_POINT ( 'NONE',  ( -6.142844459177253746, 1.156093792145113319, 5.615601928929211617 ) ) ;
#13552 = DIRECTION ( 'NONE',  ( 3.326610055774640194E-18, -1.000000000000000000, -3.608224830031754812E-16 ) ) ;
#13553 = DIRECTION ( 'NONE',  ( 1.000000000000000000, 0.000000000000000000, 0.000000000000000000 ) ) ;
#13554 = CARTESIAN_POINT ( 'NONE',  ( -1.035533905932739751, 186.9199999975965625, 9.500000000000003553 ) ) ;
#13555 = CARTESIAN_POINT ( 'NONE',  ( -1.132970084112051579, 227.7246690377758398, 5.444219334014433365 ) ) ;
#13556 = CARTESIAN_POINT ( 'NONE',  ( 2.548737910730607403, 227.7996913757372397, 8.828908791204545636 ) ) ;
#13557 = VECTOR ( 'NONE', #1412, 1000.000000000000000 ) ;
#13558 = CARTESIAN_POINT ( 'NONE',  ( -3.024391221093167825, 189.3078535938050209, 6.878255494570371553 ) ) ;
#13559 = ORIENTED_EDGE ( 'NONE', *, *, #4590, .T. ) ;
#13560 = CARTESIAN_POINT ( 'NONE',  ( 2.897581130414634077E-17, 19.99999999999999645, 11.25000000000000355 ) ) ;
#13561 = CARTESIAN_POINT ( 'NONE',  ( -7.180990026460740694, -3.384707322287537679, 31.00000000000000000 ) ) ;
#13562 = CARTESIAN_POINT ( 'NONE',  ( -4.286401442266736694, 4.198423832312983883, 24.36938304467860661 ) ) ;
#13563 = CARTESIAN_POINT ( 'NONE',  ( 0.9999196734184672142, 5.916093360767482601, 24.36725955955066425 ) ) ;
#13564 = CARTESIAN_POINT ( 'NONE',  ( 2.769757902222948154, 226.9188947913604295, 6.236235719881334738 ) ) ;
#13565 = DIRECTION ( 'NONE',  ( -0.3090169943749447867, -0.9510565162951544194, 0.000000000000000000 ) ) ;
#13566 = CARTESIAN_POINT ( 'NONE',  ( -2.500000000000000444, 1.035533905932737753, 1.649999999999999911 ) ) ;
#13567 = CARTESIAN_POINT ( 'NONE',  ( 5.747343991580192046, -1.727858744772256427, 4.000079976437387330 ) ) ;
#13568 = EDGE_CURVE ( 'NONE', #7504, #13484, #10175, .T. ) ;
#13569 = LINE ( 'NONE', #5235, #5207 ) ;
#13570 = CARTESIAN_POINT ( 'NONE',  ( -2.500000000000000444, 186.0500000000000114, 8.035533905932737753 ) ) ;
#13571 = PLANE ( 'NONE',  #5280 ) ;
#13572 = EDGE_CURVE ( 'NONE', #15526, #8395, #8179, .T. ) ;
#13573 = CARTESIAN_POINT ( 'NONE',  ( 6.176542424588109093, 0.9554180641286111886, 31.00000000000000000 ) ) ;
#13574 = CARTESIAN_POINT ( 'NONE',  ( 1.461580736456473018, -1.461580736456472573, -2.249999998907525445 ) ) ;
#13575 = CARTESIAN_POINT ( 'NONE',  ( 4.416779112813599362, 4.422345839825853275, 11.76225281721714744 ) ) ;
#13576 = DIRECTION ( 'NONE',  ( -1.000000000000000000, 3.326610055774637112E-18, 1.062480551894331163E-17 ) ) ;
#13577 = CARTESIAN_POINT ( 'NONE',  ( -6.268043809681822509E-16, 188.0499999989075093, 9.066987300000000971 ) ) ;
#13578 = CARTESIAN_POINT ( 'NONE',  ( 1.035533905932737753, 187.2499999978150811, 4.500000000000001776 ) ) ;
#13580 = EDGE_LOOP ( 'NONE', ( #2224, #5306, #6321, #4394 ) ) ;
#13579 = CARTESIAN_POINT ( 'NONE',  ( -2.066987300000000971, 188.8999999989075320, 7.856174172912944620 ) ) ;
#13581 = CARTESIAN_POINT ( 'NONE',  ( -3.632151824461103740, -4.777505256984581727, 16.99995067926686332 ) ) ;
#13582 = AXIS2_PLACEMENT_3D ( 'NONE', #5919, #8393, #13229 ) ;
#13583 = CARTESIAN_POINT ( 'NONE',  ( 6.020822430078820453, -1.681351817312314090, 12.47408542334169113 ) ) ;
#13584 = CARTESIAN_POINT ( 'NONE',  ( 0.06635618020083272617, 190.0874453959174275, 4.202409577918525763 ) ) ;
#13585 = ADVANCED_FACE ( 'NONE', ( #13891 ), #5710, .F. ) ;
#13586 = CARTESIAN_POINT ( 'NONE',  ( -1.461580736456473240, 188.5499999989075093, 5.538419263543526760 ) ) ;
#13587 = CARTESIAN_POINT ( 'NONE',  ( 3.010624175977864692, 5.190832888732285433, 17.20111757752057002 ) ) ;
#13588 = CARTESIAN_POINT ( 'NONE',  ( 0.3313399881279415204, 189.6987757587769750, 10.37797768716739988 ) ) ;
#13589 = B_SPLINE_CURVE_WITH_KNOTS ( 'NONE', 3,
 ( #8506, #2439, #11982, #12063, #12143, #4916, #6114, #10952, #12218, #50, #1317, #3552, #4755, #14775, #128, #14616, #1088, #9845 ),
 .UNSPECIFIED., .F., .F.,
 ( 4, 2, 2, 2, 2, 2, 2, 2, 4 ),
 ( 0.003131918686235978661, 0.003523310662250268930, 0.003914702638264559199, 0.004306094614278849902, 0.004697486590293139738, 0.005088878566307429574, 0.005480270542321720277, 0.005871662518336010980, 0.006263054494350300816 ),
 .UNSPECIFIED. ) ;
#13590 = CYLINDRICAL_SURFACE ( 'NONE', #8088, 2.500000000000000444 ) ;
#13591 = CARTESIAN_POINT ( 'NONE',  ( -1.524659305057740610E-16, 189.0000000000000000, 4.500000000000000000 ) ) ;
#13592 = CARTESIAN_POINT ( 'NONE',  ( 1.767766984964215471, 1.767766920968521616, -2.500000000000000444 ) ) ;
#13593 = CARTESIAN_POINT ( 'NONE',  ( -5.866984344570825627, -1.259800266528668500, 12.29931806258173488 ) ) ;
#13594 = DIRECTION ( 'NONE',  ( -1.000000000000000000, 0.000000000000000000, 0.000000000000000000 ) ) ;
#13595 = CIRCLE ( 'NONE', #12575, 1.499999999999999556 ) ;
#13596 = ORIENTED_EDGE ( 'NONE', *, *, #13677, .F. ) ;
#13597 = CARTESIAN_POINT ( 'NONE',  ( 1.461580736456472795, 188.5499999989075093, 5.538419263543527649 ) ) ;
#13598 = ORIENTED_EDGE ( 'NONE', *, *, #5981, .T. ) ;
#13599 = CARTESIAN_POINT ( 'NONE',  ( -5.330004929009483305, -2.755647751839598758, 24.23760108194402108 ) ) ;
#13600 = EDGE_LOOP ( 'NONE', ( #6407, #3680, #5727, #3599 ) ) ;
#13601 = CARTESIAN_POINT ( 'NONE',  ( -4.143041610105492545, 4.340967609746855693, 25.11397738943081848 ) ) ;
#13602 = ORIENTED_EDGE ( 'NONE', *, *, #13327, .T. ) ;
#13603 = CARTESIAN_POINT ( 'NONE',  ( -2.066987299999999195, -0.8561741729129466183, -1.899999998907525800 ) ) ;
#13604 = CARTESIAN_POINT ( 'NONE',  ( -6.172639027853106697, -0.9816353142772318296, 11.76225281721714389 ) ) ;
#13605 = CARTESIAN_POINT ( 'NONE',  ( -3.002032555434545280, 189.8710560290441265, 7.456578097359207291 ) ) ;
#13606 = CARTESIAN_POINT ( 'NONE',  ( -0.7993401192310704007, 6.199366368793674198, 25.11483246936562352 ) ) ;
#13607 = CARTESIAN_POINT ( 'NONE',  ( 1.035533905932739085, -2.500000000000000000, 1.150000000000000133 ) ) ;
#13608 = DIRECTION ( 'NONE',  ( 0.000000000000000000, -0.000000000000000000, -1.000000000000000000 ) ) ;
#13609 = CARTESIAN_POINT ( 'NONE',  ( -6.172639027853085381, -0.9816353142773684981, 24.76225281721715987 ) ) ;
#13610 = CARTESIAN_POINT ( 'NONE',  ( 1.461580736456473018, -1.461580736456472573, 0.1500000010924746052 ) ) ;
#13611 = EDGE_CURVE ( 'NONE', #10768, #2588, #12339, .T. ) ;
#13612 = CYLINDRICAL_SURFACE ( 'NONE', #14725, 1.000000000000000000 ) ;
#13613 = CARTESIAN_POINT ( 'NONE',  ( -1.826734563482391938, 226.5243062390148623, 5.073637952221710101 ) ) ;
#13614 = ORIENTED_EDGE ( 'NONE', *, *, #14182, .F. ) ;
#13615 = PRODUCT_DEFINITION ( 'UNKNOWN', '', #4771, #3074 ) ;
#13616 = ORIENTED_EDGE ( 'NONE', *, *, #12447, .F. ) ;
#13617 = ORIENTED_EDGE ( 'NONE', *, *, #9643, .T. ) ;
#13618 = CARTESIAN_POINT ( 'NONE',  ( 5.931793676715097163, -0.9035324301688445470, 30.73760108194402818 ) ) ;
#13619 = CARTESIAN_POINT ( 'NONE',  ( 0.07162589071487505954, 189.0001276426230561, 4.501026264287848910 ) ) ;
#13620 = ORIENTED_EDGE ( 'NONE', *, *, #6297, .F. ) ;
#13621 = CARTESIAN_POINT ( 'NONE',  ( -0.7995298244854599501, -5.947211616899247488, 5.614560146198585677 ) ) ;
#13622 = CARTESIAN_POINT ( 'NONE',  ( 2.082642335314403343E-14, -6.000000000000000888, 32.00000000000000000 ) ) ;
#13623 = CARTESIAN_POINT ( 'NONE',  ( 2.817313151351004574, -5.579000502529524397, 24.36936067245787996 ) ) ;
#13624 = CARTESIAN_POINT ( 'NONE',  ( 5.903472034603510110, -2.056448723545162505, 29.99991780678443476 ) ) ;
#13625 = CARTESIAN_POINT ( 'NONE',  ( -1.767766952966369098, 184.9999999978150527, 5.232233047033630235 ) ) ;
#13626 = DIRECTION ( 'NONE',  ( 0.000000000000000000, 0.000000000000000000, 1.000000000000000000 ) ) ;
#13627 = CARTESIAN_POINT ( 'NONE',  ( -4.416678568553742856, 4.422441866694219570, 11.23763026556121858 ) ) ;
#13628 = CARTESIAN_POINT ( 'NONE',  ( -1.050320854595332420E-16, 188.2000000000000171, 4.500000000000000000 ) ) ;
#13629 = DIRECTION ( 'NONE',  ( 0.000000000000000000, -1.000000000000000000, 0.000000000000000000 ) ) ;
#13630 = CARTESIAN_POINT ( 'NONE',  ( -5.929230630780102373E-16, 186.1699999975965625, 9.500000000000001776 ) ) ;
#13631 = CARTESIAN_POINT ( 'NONE',  ( -1.724657202313207849, 227.9349080091615178, 6.051401474621576071 ) ) ;
#13632 = CARTESIAN_POINT ( 'NONE',  ( -2.051698115976866355, 227.9946287341323057, 9.402281653761695779 ) ) ;
#13633 = CARTESIAN_POINT ( 'NONE',  ( -2.022860936364483386, 188.9999999987646788, 8.476761716666477042 ) ) ;
#13634 = ORIENTED_EDGE ( 'NONE', *, *, #7980, .F. ) ;
#13635 = CARTESIAN_POINT ( 'NONE',  ( -5.648559266344497232, 2.676764518775994528, 17.38603820591928439 ) ) ;
#13636 = CARTESIAN_POINT ( 'NONE',  ( 3.159612573729244200, -5.393342049074621336, 10.69973484982323697 ) ) ;
#13637 = CARTESIAN_POINT ( 'NONE',  ( 0.9999505860954052139, -6.169489349035797154, 11.63105903165811839 ) ) ;
#13638 = CARTESIAN_POINT ( 'NONE',  ( 5.649053410273044307, 2.675685104943319459, 30.38482219624157565 ) ) ;
#13639 = CARTESIAN_POINT ( 'NONE',  ( 1.189709685105988513, 228.1759518697011231, 9.935475612313785732 ) ) ;
#13640 = FACE_BOUND ( 'NONE', #7662, .T. ) ;
#13641 = CARTESIAN_POINT ( 'NONE',  ( 2.500000000000000444, -1.035533905932737309, 1.250000000000000222 ) ) ;
#13642 = CARTESIAN_POINT ( 'NONE',  ( -4.435347140101219665, 4.403429997944324548, 24.36939309276499799 ) ) ;
#13643 = PRODUCT_DEFINITION_FORMATION_WITH_SPECIFIED_SOURCE ( 'ANY', '', #13002, .NOT_KNOWN. ) ;
#13644 = CARTESIAN_POINT ( 'NONE',  ( 5.531757352715557019, 2.326874507723430519, 5.873806827147107334 ) ) ;
#13645 = CARTESIAN_POINT ( 'NONE',  ( -1.035533905932737975, 185.8500000000000227, 4.500000000000000888 ) ) ;
#13646 = FACE_BOUND ( 'NONE', #10728, .T. ) ;
#13647 = VECTOR ( 'NONE', #12122, 1000.000000000000114 ) ;
#13648 = CARTESIAN_POINT ( 'NONE',  ( 0.3253281796544252868, 227.6173729869818771, 5.134342219554626219 ) ) ;
#13649 = CARTESIAN_POINT ( 'NONE',  ( -1.461580736456472795, 1.461580736456472795, -2.649999998907524912 ) ) ;
#13650 = CARTESIAN_POINT ( 'NONE',  ( 6.105747081304222945, -1.338335777572041474, 25.30026515017674882 ) ) ;
#13651 = DIRECTION ( 'NONE',  ( -1.049359643968190670E-17, -2.775557561562888393E-16, 1.000000000000000000 ) ) ;
#13652 = CARTESIAN_POINT ( 'NONE',  ( -1.767766952966369098, 184.2999999999999829, 5.232233047033630235 ) ) ;
#13653 = CARTESIAN_POINT ( 'NONE',  ( -5.531623157106109190, -2.327208526676572298, 18.87364704684421923 ) ) ;
#13654 = AXIS2_PLACEMENT_3D ( 'NONE', #8479, #8308, #11953 ) ;
#13656 = VERTEX_POINT ( 'NONE', #5787 ) ;
#13655 = CARTESIAN_POINT ( 'NONE',  ( 2.066987300000000083, 187.6499999989075320, 7.000000000000000000 ) ) ;
#13657 = ADVANCED_FACE ( 'NONE', ( #607 ), #12852, .T. ) ;
#13658 = FACE_BOUND ( 'NONE', #4198, .T. ) ;
#13659 = AXIS2_PLACEMENT_3D ( 'NONE', #8609, #3732, #4781 ) ;
#13660 = CARTESIAN_POINT ( 'NONE',  ( 5.931828553037973961, -0.9033193133619329407, 5.261943240031468960 ) ) ;
#13661 = ADVANCED_FACE ( 'NONE', ( #10633, #5479 ), #4273, .F. ) ;
#13662 = CARTESIAN_POINT ( 'NONE',  ( -5.999999999999999112, 195.9172377311516016, 6.220370292208425411 ) ) ;
#13663 = DIRECTION ( 'NONE',  ( -0.9510565162951545304, 0.3090169943749447867, 0.000000000000000000 ) ) ;
#13664 = CARTESIAN_POINT ( 'NONE',  ( 2.500000000000000000, 3.061616997868383141E-16, 0.5000000000000000000 ) ) ;
#13665 = CARTESIAN_POINT ( 'NONE',  ( 2.378934927046848724, 189.7843313986748512, 9.198200349355834859 ) ) ;
#13666 = PLANE ( 'NONE',  #4530 ) ;
#13667 = CARTESIAN_POINT ( 'NONE',  ( 2.605749592490243405, 189.8045552418427064, 8.848848054815309894 ) ) ;
#13669 = CARTESIAN_POINT ( 'NONE',  ( 5.985119669071172765, -1.805077827356371900, 23.50008258189710020 ) ) ;
#13668 = AXIS2_PLACEMENT_3D ( 'NONE', #8694, #2556, #1353 ) ;
#13670 = LINE ( 'NONE', #3887, #11594 ) ;
#13671 = CARTESIAN_POINT ( 'NONE',  ( 4.286401442266389417, 4.198423832313341819, 24.36763921416088863 ) ) ;
#13672 = CARTESIAN_POINT ( 'NONE',  ( -5.620879908643967582, 2.102487719021896684, 12.47377823943291375 ) ) ;
#13673 = ORIENTED_EDGE ( 'NONE', *, *, #12988, .F. ) ;
#13674 = CARTESIAN_POINT ( 'NONE',  ( -1.592421940838084637E-16, 188.6499999989075320, 4.933012699999999029 ) ) ;
#13675 = ORIENTED_EDGE ( 'NONE', *, *, #6103, .F. ) ;
#13676 = DIRECTION ( 'NONE',  ( 0.000000000000000000, 0.000000000000000000, 1.000000000000000000 ) ) ;
#13677 = EDGE_CURVE ( 'NONE', #14887, #13744, #10323, .T. ) ;
#13678 = ORIENTED_EDGE ( 'NONE', *, *, #6410, .T. ) ;
#13679 = CYLINDRICAL_SURFACE ( 'NONE', #11145, 2.500000000000000000 ) ;
#13680 = CARTESIAN_POINT ( 'NONE',  ( 1.035533905932737975, 185.7500000000000000, 4.500000000000001776 ) ) ;
#13681 = EDGE_LOOP ( 'NONE', ( #3738, #9822 ) ) ;
#13682 = VECTOR ( 'NONE', #7717, 1000.000000000000114 ) ;
#13683 =( GEOMETRIC_REPRESENTATION_CONTEXT ( 3 ) GLOBAL_UNCERTAINTY_ASSIGNED_CONTEXT ( ( #11877 ) ) GLOBAL_UNIT_ASSIGNED_CONTEXT ( ( #13761, #8849, #6696 ) ) REPRESENTATION_CONTEXT ( 'NONE', 'WORKASPACE' ) );
#13684 = CARTESIAN_POINT ( 'NONE',  ( 0.8561741729129463963, -2.066987299999999195, -1.699999998907525400 ) ) ;
#13685 = ADVANCED_FACE ( 'NONE', ( #12934 ), #3080, .F. ) ;
#13686 = CARTESIAN_POINT ( 'NONE',  ( -1.035533905932737753, 2.500000000000000444, -1.649999999999999911 ) ) ;
#13687 = DIRECTION ( 'NONE',  ( 0.5877852522924802425, -0.8090169943749422332, 0.000000000000000000 ) ) ;
#13688 = CARTESIAN_POINT ( 'NONE',  ( -6.877907531704918753E-16, 189.0499999989075093, 9.066987300000000971 ) ) ;
#13689 = CARTESIAN_POINT ( 'NONE',  ( 1.767766952966368654, 1.767766952966369098, -1.000000000000000000 ) ) ;
#13690 = CARTESIAN_POINT ( 'NONE',  ( -4.006441409774819995, 4.467329318258138393, 17.20111757752057713 ) ) ;
#13691 = ITEM_DEFINED_TRANSFORMATION ( 'NONE', 'NONE', #2480,  #14201 ) ;
#13692 = CARTESIAN_POINT ( 'NONE',  ( 4.195795028115099079, -4.289273350251257888, 31.50428920362021046 ) ) ;
#13693 = CARTESIAN_POINT ( 'NONE',  ( -0.8561741729129455081, 2.066987299999999639, 0.5000000010924747773 ) ) ;
#13694 = CARTESIAN_POINT ( 'NONE',  ( -6.142908455506956855, 1.155755562475991427, 30.38482219624157565 ) ) ;
#13695 = CARTESIAN_POINT ( 'NONE',  ( -0.7777163206635004933, 228.2226383035325057, 10.07273956871427956 ) ) ;
#13696 = APPLICATION_CONTEXT ( 'automotive_design' ) ;
#13697 = ORIENTED_EDGE ( 'NONE', *, *, #92, .T. ) ;
#13698 = VECTOR ( 'NONE', #5251, 1000.000000000000114 ) ;
#13699 = ORIENTED_EDGE ( 'NONE', *, *, #15250, .F. ) ;
#13700 = EDGE_LOOP ( 'NONE', ( #9684, #10207 ) ) ;
#13701 = ORIENTED_EDGE ( 'NONE', *, *, #7740, .T. ) ;
#13702 = CARTESIAN_POINT ( 'NONE',  ( 4.416397290909912954, 4.422724436066427067, 4.736203831591939917 ) ) ;
#13703 = EDGE_LOOP ( 'NONE', ( #10304, #9459 ) ) ;
#13704 = CARTESIAN_POINT ( 'NONE',  ( -0.6144377077729846759, -5.969178481556066451, 4.200339668577364627 ) ) ;
#13705 = EDGE_CURVE ( 'NONE', #14110, #9498, #5056, .T. ) ;
#13706 = DIRECTION ( 'NONE',  ( -0.000000000000000000, 1.000000000000000000, -0.000000000000000000 ) ) ;
#13707 = CARTESIAN_POINT ( 'NONE',  ( -2.817313151351206635, 5.579000502529421368, 31.13237410716304865 ) ) ;
#13708 =( GEOMETRIC_REPRESENTATION_CONTEXT ( 3 ) GLOBAL_UNCERTAINTY_ASSIGNED_CONTEXT ( ( #8404 ) ) GLOBAL_UNIT_ASSIGNED_CONTEXT ( ( #775, #8509, #14621 ) ) REPRESENTATION_CONTEXT ( 'NONE', 'WORKASPACE' ) );
#13709 = CARTESIAN_POINT ( 'NONE',  ( 5.770288754215132876, -2.404361317819945221, 30.12618035954928075 ) ) ;
#13710 = CARTESIAN_POINT ( 'NONE',  ( 2.500000000000000444, 187.0999999978150754, 7.000000000000000000 ) ) ;
#13711 = FILL_AREA_STYLE ('',( #3182 ) ) ;
#13712 = DIRECTION ( 'NONE',  ( 0.000000000000000000, 0.000000000000000000, -1.000000000000000000 ) ) ;
#13713 = AXIS2_PLACEMENT_3D ( 'NONE', #14108, #591, #5769 ) ;
#13714 = CARTESIAN_POINT ( 'NONE',  ( 3.311576095066511183, 5.004818610361351006, 10.52622176056705072 ) ) ;
#13715 = CARTESIAN_POINT ( 'NONE',  ( -9.750000000000003553, 66.00000000000000000, -3.401296724241641415E-14 ) ) ;
#13716 = EDGE_CURVE ( 'NONE', #6866, #10284, #13088, .T. ) ;
#13717 = CARTESIAN_POINT ( 'NONE',  ( -1.767766952966369765, 186.8699999975965511, 8.767766952966368876 ) ) ;
#13718 = CARTESIAN_POINT ( 'NONE',  ( -0.7013870287959992345, 228.8704690996177646, 8.753355264767147759 ) ) ;
#13719 = CARTESIAN_POINT ( 'NONE',  ( -2.976076845141470972, 227.1639356932526539, 6.957862568523350610 ) ) ;
#13720 = CARTESIAN_POINT ( 'NONE',  ( -2.593495354050888491, 189.9612784629288456, 5.721711197761079504 ) ) ;
#13721 = AXIS2_PLACEMENT_3D ( 'NONE', #6016, #7210, #12050 ) ;
#13722 = VERTEX_POINT ( 'NONE', #13251 ) ;
#13723 = CARTESIAN_POINT ( 'NONE',  ( 0.000000000000000000, 0.000000000000000000, 36.00000000000000711 ) ) ;
#13724 = CYLINDRICAL_SURFACE ( 'NONE', #6108, 1.499999999999999556 ) ;
#13725 = CARTESIAN_POINT ( 'NONE',  ( -0.5043776560897343941, 6.230795654995838539, 5.873374762960125395 ) ) ;
#13726 = CARTESIAN_POINT ( 'NONE',  ( 0.6156307853271528741, 5.969051238897232103, 25.29870573410679668 ) ) ;
#13727 = EDGE_CURVE ( 'NONE', #8841, #6081, #4018, .T. ) ;
#13728 = B_SPLINE_CURVE_WITH_KNOTS ( 'NONE', 3,
 ( #15488, #835, #5547, #5857, #6974, #2024, #910, #10395, #10703, #1869, #2178, #8086, #3150, #4266, #6743, #7049, #14195, #11884, #9354 ),
 .UNSPECIFIED., .F., .F.,
 ( 4, 3, 3, 3, 3, 3, 4 ),
 ( 0.0005509418849372115044, 0.0005730732227554590505, 0.0006075432786058860765, 0.0006294361076369635061, 0.0006629275523618718491, 0.0006964354412241015486, 0.0006994975975014303734 ),
 .UNSPECIFIED. ) ;
#13729 = CARTESIAN_POINT ( 'NONE',  ( 1.569541343170871794, 228.1129751185468706, 9.750325026063840994 ) ) ;
#13730 = EDGE_CURVE ( 'NONE', #12581, #12174, #11025, .T. ) ;
#13731 = CARTESIAN_POINT ( 'NONE',  ( -2.997753866155750568, -5.484939622623882016, 31.61560192892922672 ) ) ;
#13732 = CARTESIAN_POINT ( 'NONE',  ( -1.767766952966369098, 1.767766952966369098, 2.400000000000000355 ) ) ;
#13733 = CARTESIAN_POINT ( 'NONE',  ( -7.420008617947670970E-16, 188.5999999999999943, 9.500000000000001776 ) ) ;
#13734 = CARTESIAN_POINT ( 'NONE',  ( -2.841041022017330331, -5.567186575787293812, 30.73774718278283302 ) ) ;
#13735 = CARTESIAN_POINT ( 'NONE',  ( 1.035533905932737753, 187.3499999999999659, 4.500000000000000888 ) ) ;
#13736 = CARTESIAN_POINT ( 'NONE',  ( -1.035533905932738197, -2.500000000000000000, -2.049999997815050268 ) ) ;
#13737 = CARTESIAN_POINT ( 'NONE',  ( 0.4220225674029139951, 227.6236908799334344, 5.152588654748359254 ) ) ;
#13738 = CARTESIAN_POINT ( 'NONE',  ( -2.066987299999999639, 0.8561741729129455081, -1.799999998907525045 ) ) ;
#13739 = CARTESIAN_POINT ( 'NONE',  ( 2.500000000000000444, -1.035533905932737309, -2.649999997815050357 ) ) ;
#13740 = LINE ( 'NONE', #5082, #12651 ) ;
#13741 = CARTESIAN_POINT ( 'NONE',  ( 2.500000000000000444, 184.7999999999999829, 7.000000000000000000 ) ) ;
#13742 = CARTESIAN_POINT ( 'NONE',  ( -2.668367453516831134, 5.373994336898032742, 18.13239388001634467 ) ) ;
#13744 = VERTEX_POINT ( 'NONE', #9443 ) ;
#13743 = CARTESIAN_POINT ( 'NONE',  ( -1.461580736456473018, 187.1499999989075320, 5.538419263543527649 ) ) ;
#13745 = CARTESIAN_POINT ( 'NONE',  ( 4.286401442266532413, 4.198423832313196158, 5.000000000000004441 ) ) ;
#13746 = LINE ( 'NONE', #2614, #6049 ) ;
#13747 = CARTESIAN_POINT ( 'NONE',  ( 0.000000000000000000, 229.2449477060184222, 9.834870838912449287 ) ) ;
#13748 = LINE ( 'NONE', #1574, #13698 ) ;
#13749 = CARTESIAN_POINT ( 'NONE',  ( 1.955037902524143778, 188.9999999998599378, 8.565347031248222720 ) ) ;
#13750 = DIRECTION ( 'NONE',  ( 0.000000000000000000, 1.000000000000000000, 0.000000000000000000 ) ) ;
#13751 = CARTESIAN_POINT ( 'NONE',  ( 0.7847739342500663628, 189.7061529762492569, 10.28987046638656544 ) ) ;
#13752 = CARTESIAN_POINT ( 'NONE',  ( -3.011385983131386723, 5.190390249166400238, 30.20047945897283270 ) ) ;
#13753 = CARTESIAN_POINT ( 'NONE',  ( 0.8499999999999896527, -0.3999999999999958589, 2.619018321873339161 ) ) ;
#13754 = DIRECTION ( 'NONE',  ( 0.000000000000000000, 0.000000000000000000, 1.000000000000000000 ) ) ;
#13755 = ORIENTED_EDGE ( 'NONE', *, *, #4732, .T. ) ;
#13756 = CARTESIAN_POINT ( 'NONE',  ( -6.098637220230962441E-17, 187.0499999989075093, 4.933012699999999029 ) ) ;
#13757 = VERTEX_POINT ( 'NONE', #1155 ) ;
#13758 = LINE ( 'NONE', #14807, #9873 ) ;
#13759 = ORIENTED_EDGE ( 'NONE', *, *, #11965, .T. ) ;
#13760 = DIRECTION ( 'NONE',  ( 0.8090169943749421222, 0.5877852522924802425, 0.000000000000000000 ) ) ;
#13761 =( LENGTH_UNIT ( ) NAMED_UNIT ( * ) SI_UNIT ( .MILLI., .METRE. ) );
#13762 = ORIENTED_EDGE ( 'NONE', *, *, #14457, .T. ) ;
#13763 = CARTESIAN_POINT ( 'NONE',  ( 2.066987299999999639, 0.8561741729129456191, 0.1000000010924746996 ) ) ;
#13764 = CARTESIAN_POINT ( 'NONE',  ( -2.997753866155803415, 5.484939622623852706, 4.384398071070799929 ) ) ;
#13765 = CARTESIAN_POINT ( 'NONE',  ( -2.267268076141566002, 189.9944061229849979, 5.253861789810808425 ) ) ;
#13766 = FACE_OUTER_BOUND ( 'NONE', #12561, .T. ) ;
#13767 = CARTESIAN_POINT ( 'NONE',  ( -2.500000000000000000, -1.035533905932739307, -2.250000000000000444 ) ) ;
#13768 = CARTESIAN_POINT ( 'NONE',  ( 1.767766952966369320, -1.767766952966368654, -1.200000000000000178 ) ) ;
#13769 = DIRECTION ( 'NONE',  ( -0.3090169943749579429, 0.9510565162951502005, 0.000000000000000000 ) ) ;
#13770 = EDGE_CURVE ( 'NONE', #11747, #8394, #3046, .T. ) ;
#13771 = CARTESIAN_POINT ( 'NONE',  ( -1.767766952966369765, 186.9000000000000057, 8.767766952966368876 ) ) ;
#13772 = CARTESIAN_POINT ( 'NONE',  ( 0.8561741729129463963, -2.066987299999999195, -0.6999999989075250673 ) ) ;
#13773 = CARTESIAN_POINT ( 'NONE',  ( 0.000000000000000000, 6.250000000000000888, 32.00000000000000000 ) ) ;
#13774 = EDGE_CURVE ( 'NONE', #9246, #12662, #4286, .T. ) ;
#13775 = ORIENTED_EDGE ( 'NONE', *, *, #1802, .T. ) ;
#13776 = AXIS2_PLACEMENT_3D ( 'NONE', #6117, #2758, #10954 ) ;
#13777 = VERTEX_POINT ( 'NONE', #8252 ) ;
#13778 = ORIENTED_EDGE ( 'NONE', *, *, #8137, .T. ) ;
#13779 = CARTESIAN_POINT ( 'NONE',  ( -2.500000000000000000, 0.000000000000000000, 1.000000002184949777 ) ) ;
#13780 = CARTESIAN_POINT ( 'NONE',  ( 5.616089948629690021, 2.743103014345625645, 4.495630303198470124 ) ) ;
#13781 = ORIENTED_EDGE ( 'NONE', *, *, #748, .T. ) ;
#13782 = CYLINDRICAL_SURFACE ( 'NONE', #14720, 1.499999999999999556 ) ;
#13783 = CARTESIAN_POINT ( 'NONE',  ( 0.1306497350717528982, -6.000000000000000000, 30.00000000000000355 ) ) ;
#13784 = CARTESIAN_POINT ( 'NONE',  ( -4.344502777243570257, 4.493369211529226526, 31.50389213124969601 ) ) ;
#13785 = FACE_OUTER_BOUND ( 'NONE', #1369, .T. ) ;
#13786 = CARTESIAN_POINT ( 'NONE',  ( -2.500000000000000444, 187.5499999978150356, 8.035533905932737753 ) ) ;
#13787 = VECTOR ( 'NONE', #10939, 1000.000000000000114 ) ;
#13788 = CARTESIAN_POINT ( 'NONE',  ( 1.767766952966369320, -1.767766952966368654, 1.206999999978150440 ) ) ;
#13789 = CARTESIAN_POINT ( 'NONE',  ( -4.435347140101170815, 4.403429997944372509, 17.99999999999998934 ) ) ;
#13790 =( LENGTH_UNIT ( ) NAMED_UNIT ( * ) SI_UNIT ( .MILLI., .METRE. ) );
#13791 = CARTESIAN_POINT ( 'NONE',  ( -1.035533905932737753, 185.8199999975965682, 4.500000000000000888 ) ) ;
#13792 = CARTESIAN_POINT ( 'NONE',  ( -1.964265005259087538, 228.3667458257928047, 7.298573719466742382 ) ) ;
#13793 = CARTESIAN_POINT ( 'NONE',  ( -2.548338711267991386, 226.7802694665861338, 5.827877803219676522 ) ) ;
#13794 = ORIENTED_EDGE ( 'NONE', *, *, #210, .F. ) ;
#13795 = CARTESIAN_POINT ( 'NONE',  ( 1.767766952966369320, -1.767766952966368654, 0.5000000021849496656 ) ) ;
#13796 = ORIENTED_EDGE ( 'NONE', *, *, #9412, .F. ) ;
#13797 = DIRECTION ( 'NONE',  ( 0.000000000000000000, 0.000000000000000000, -1.000000000000000000 ) ) ;
#13798 = CARTESIAN_POINT ( 'NONE',  ( -5.558508435838135142, 2.857531096719037489, 24.49999999999999289 ) ) ;
#13799 = CARTESIAN_POINT ( 'NONE',  ( -2.668367453516892418, 5.373994336898002544, 24.36763921416089218 ) ) ;
#13800 = CARTESIAN_POINT ( 'NONE',  ( -1.965116437629976787E-16, 189.6999999978150697, 4.500000000000000000 ) ) ;
#13801 = FACE_OUTER_BOUND ( 'NONE', #6814, .T. ) ;
#13802 = CARTESIAN_POINT ( 'NONE',  ( -3.159082487394730521, -5.393634094348361607, 31.79954462468843346 ) ) ;
#13803 = EDGE_CURVE ( 'NONE', #4625, #15036, #9603, .T. ) ;
#13804 = CARTESIAN_POINT ( 'NONE',  ( 4.592425496802573972E-16, -2.500000000000000000, 1.899999999999999911 ) ) ;
#13805 = CARTESIAN_POINT ( 'NONE',  ( 2.848727059636034120, 5.281416301279857173, 4.385574784280629856 ) ) ;
#13806 = VECTOR ( 'NONE', #1891, 1000.000000000000000 ) ;
#13807 = CARTESIAN_POINT ( 'NONE',  ( 1.035533905932737753, 188.9500000000000171, 4.500000000000001776 ) ) ;
#13808 = CARTESIAN_POINT ( 'NONE',  ( -1.767766952966369320, 187.5000000000000000, 5.232233047033630235 ) ) ;
#13809 = CARTESIAN_POINT ( 'NONE',  ( -1.051851325171203388, 227.7069327454752283, 5.392995910236884960 ) ) ;
#13810 = CARTESIAN_POINT ( 'NONE',  ( -2.500000000000000000, 0.000000000000000000, 2.500000000000000000 ) ) ;
#13811 = EDGE_CURVE ( 'NONE', #3723, #8478, #15195, .T. ) ;
#13812 = CARTESIAN_POINT ( 'NONE',  ( 3.883716939929014345, 4.898343590941228065, 12.47359571723299965 ) ) ;
#13813 = CARTESIAN_POINT ( 'NONE',  ( 2.066987299999999639, 0.8561741729129456191, 0.9000000010924746885 ) ) ;
#13814 = CARTESIAN_POINT ( 'NONE',  ( 1.035533905932738419, 184.6500000000000057, 9.500000000000003553 ) ) ;
#13815 = CARTESIAN_POINT ( 'NONE',  ( -4.286401442266689621, 4.198423832313033621, 18.13064961348853998 ) ) ;
#13817 = VERTEX_POINT ( 'NONE', #6024 ) ;
#13816 = CARTESIAN_POINT ( 'NONE',  ( -1.016439536705160407E-17, 186.2499999989074979, 4.933012699999999029 ) ) ;
#13818 = FACE_OUTER_BOUND ( 'NONE', #14882, .T. ) ;
#13819 = DIRECTION ( 'NONE',  ( 1.000000000000000000, 0.000000000000000000, 0.000000000000000000 ) ) ;
#13820 = B_SPLINE_CURVE_WITH_KNOTS ( 'NONE', 3,
 ( #9554, #950, #14392, #8123, #9314, #5585, #15283, #2218, #1030, #13207, #5737, #10660, #12961, #8283, #2061, #11768, #12879, #10581 ),
 .UNSPECIFIED., .F., .F.,
 ( 4, 2, 2, 2, 2, 2, 2, 2, 4 ),
 ( 0.000000000000000000, 0.0003914898357794966278, 0.0007829796715589932557, 0.001174469507338489829, 0.001565959343117987596, 0.001957449178897484494, 0.002348939014676980960, 0.002740428850456477425, 0.003131918686235973890 ),
 .UNSPECIFIED. ) ;
#13821 = VECTOR ( 'NONE', #4758, 1000.000000000000000 ) ;
#13822 = CARTESIAN_POINT ( 'NONE',  ( 0.000000000000000000, 215.7452399395091049, 13.29567785264566027 ) ) ;
#13823 = CARTESIAN_POINT ( 'NONE',  ( 2.978694808295341279, 189.3199727616403720, 6.623693945629629987 ) ) ;
#13824 = CARTESIAN_POINT ( 'NONE',  ( 0.04451878633413008934, -0.3999999999999923617, -2.535225719870653815 ) ) ;
#13825 = CARTESIAN_POINT ( 'NONE',  ( -5.487348639458879518, -2.428538342494442226, 5.800222173838808892 ) ) ;
#13826 = CARTESIAN_POINT ( 'NONE',  ( 0.000000000000000000, 189.6977690162252657, 10.38967773564543862 ) ) ;
#13827 = CARTESIAN_POINT ( 'NONE',  ( 5.558508435838229289, -2.857531096718852748, 5.132374107163055754 ) ) ;
#13828 = DIRECTION ( 'NONE',  ( -0.000000000000000000, 1.000000000000000000, -0.000000000000000000 ) ) ;
#13829 = CARTESIAN_POINT ( 'NONE',  ( -13.50000000000000000, 0.000000000000000000, 2.000000000000002220 ) ) ;
#13830 = VERTEX_POINT ( 'NONE', #4911 ) ;
#13831 = CARTESIAN_POINT ( 'NONE',  ( -0.8561741729129455081, 185.4999999989075548, 4.933012699999999029 ) ) ;
#13832 = B_SPLINE_CURVE_WITH_KNOTS ( 'NONE', 3,
 ( #14318, #9487, #2077, #3425, #11782, #11708, #8296, #6950, #3351, #3512, #15457, #884, #965, #10523, #5752, #6874, #10596, #7102 ),
 .UNSPECIFIED., .F., .F.,
 ( 4, 2, 2, 2, 2, 2, 2, 2, 4 ),
 ( 0.000000000000000000, 0.0003914904498596245754, 0.0007829808997192491508, 0.001174471349578873726, 0.001565961799438498302, 0.001957452249298123094, 0.002348942699157747453, 0.002740433149017371811, 0.003131923598876996603 ),
 .UNSPECIFIED. ) ;
#13833 = ORIENTED_EDGE ( 'NONE', *, *, #2292, .F. ) ;
#13834 = CARTESIAN_POINT ( 'NONE',  ( 0.000000000000000000, 0.000000000000000000, 0.000000000000000000 ) ) ;
#13835 = VECTOR ( 'NONE', #1364, 1000.000000000000114 ) ;
#13836 = ORIENTED_EDGE ( 'NONE', *, *, #4036, .T. ) ;
#13837 = DIRECTION ( 'NONE',  ( 0.5877852522924802425, -0.8090169943749422332, 0.000000000000000000 ) ) ;
#13838 = DIRECTION ( 'NONE',  ( 0.000000000000000000, 0.000000000000000000, 1.000000000000000000 ) ) ;
#13839 = ORIENTED_EDGE ( 'NONE', *, *, #1999, .F. ) ;
#13840 = CARTESIAN_POINT ( 'NONE',  ( -2.782769401326126157, -5.315896561274875864, 5.504289203620205129 ) ) ;
#13841 = CARTESIAN_POINT ( 'NONE',  ( 2.500000000000000000, 3.061616997868383141E-16, -1.900000000000000133 ) ) ;
#13842 = DIRECTION ( 'NONE',  ( -0.000000000000000000, -1.000000000000000000, -0.000000000000000000 ) ) ;
#13843 = CARTESIAN_POINT ( 'NONE',  ( -2.500000000000000000, -0.4783542904563624076, 1.823096990497731884 ) ) ;
#13844 = FACE_BOUND ( 'NONE', #12408, .T. ) ;
#13845 = CARTESIAN_POINT ( 'NONE',  ( -2.500000000000000000, 0.000000000000000000, -0.5999999978150503122 ) ) ;
#13846 = CARTESIAN_POINT ( 'NONE',  ( -1.461580736456472351, -1.461580736456473018, -1.649999998907525356 ) ) ;
#13847 = CARTESIAN_POINT ( 'NONE',  ( 2.782468714962335277, 5.316055268221454355, 12.00389795015984795 ) ) ;
#13848 = ORIENTED_EDGE ( 'NONE', *, *, #12828, .F. ) ;
#13849 = ORIENTED_EDGE ( 'NONE', *, *, #15126, .T. ) ;
#13850 = VERTEX_POINT ( 'NONE', #2350 ) ;
#13851 = CARTESIAN_POINT ( 'NONE',  ( 3.158296126777787372, -5.394094919772115304, 18.79887838423338309 ) ) ;
#13852 = LINE ( 'NONE', #12585, #1983 ) ;
#13853 = ORIENTED_EDGE ( 'NONE', *, *, #13774, .T. ) ;
#13854 = AXIS2_PLACEMENT_3D ( 'NONE', #522, #12538, #3940 ) ;
#13855 = CARTESIAN_POINT ( 'NONE',  ( 5.935543223013881153, -0.8771126767605277319, 18.13064961348853998 ) ) ;
#13856 = ADVANCED_FACE ( 'NONE', ( #13329 ), #7220, .T. ) ;
#13857 = CARTESIAN_POINT ( 'NONE',  ( -2.500000000000000000, 0.000000000000000000, 1.000000002184949777 ) ) ;
#13858 = DIRECTION ( 'NONE',  ( 0.000000000000000000, 0.000000000000000000, 1.000000000000000000 ) ) ;
#13859 = CARTESIAN_POINT ( 'NONE',  ( 6.021135683317704768, -1.680226122398187583, 30.02622717124732077 ) ) ;
#13860 = CARTESIAN_POINT ( 'NONE',  ( 1.767766952966368432, 186.9999999978150527, 8.767766952966368876 ) ) ;
#13861 = CARTESIAN_POINT ( 'NONE',  ( 5.935543223013869607, -0.8771126767605967878, 11.49999999999998224 ) ) ;
#13862 = CARTESIAN_POINT ( 'NONE',  ( 3.000000000000000000, 3.673940397442059868E-16, 5.000000000000004441 ) ) ;
#13863 = DIRECTION ( 'NONE',  ( 6.982962677686266711E-15, 0.000000000000000000, -1.000000000000000000 ) ) ;
#13864 = CARTESIAN_POINT ( 'NONE',  ( -2.500000000000000444, 186.8199999975965397, 8.035533905932737753 ) ) ;
#13865 = CARTESIAN_POINT ( 'NONE',  ( -1.973877840180719989, 228.3455757694837303, 7.237433389386023208 ) ) ;
#13866 = CARTESIAN_POINT ( 'NONE',  ( -0.4900172623563870955, 226.3376062179358996, 4.523300904952406221 ) ) ;
#13867 = EDGE_LOOP ( 'NONE', ( #4316, #1800, #15451, #2272 ) ) ;
#13868 = EDGE_CURVE ( 'NONE', #13014, #8921, #7612, .T. ) ;
#13869 = CARTESIAN_POINT ( 'NONE',  ( 4.286401442266591921, -4.198423832313133985, 4.867606119983652668 ) ) ;
#13870 = VERTEX_POINT ( 'NONE', #7522 ) ;
#13871 = CARTESIAN_POINT ( 'NONE',  ( 4.416397290909979567, -4.422724436066356901, 5.263796168408045872 ) ) ;
#13872 = EDGE_CURVE ( 'NONE', #6892, #8289, #3996, .T. ) ;
#13873 = DIRECTION ( 'NONE',  ( -0.5877852522924685852, -0.8090169943749507819, 0.000000000000000000 ) ) ;
#13874 = CARTESIAN_POINT ( 'NONE',  ( 1.000049271338558032, -6.169473353325540366, 11.36969612704552546 ) ) ;
#13875 = CARTESIAN_POINT ( 'NONE',  ( 0.7988914244720274338, 5.947301735519258337, 23.88456289168618341 ) ) ;
#13876 = CARTESIAN_POINT ( 'NONE',  ( -1.016439536705160407E-17, 228.2551366889529731, 10.16828399152529272 ) ) ;
#13877 = CARTESIAN_POINT ( 'NONE',  ( 2.782468714962265555, -5.316055268221492547, 23.99610204984018580 ) ) ;
#13878 = CARTESIAN_POINT ( 'NONE',  ( 2.500000000000000000, 3.061616997868383141E-16, 2.100000000000000089 ) ) ;
#13879 = CARTESIAN_POINT ( 'NONE',  ( -1.265664690411614835E-16, 2.066987299999999639, -1.949999998907525622 ) ) ;
#13880 = CARTESIAN_POINT ( 'NONE',  ( -3.107583187530371660, -5.133966411712722611, 31.87380682714712066 ) ) ;
#13881 = SURFACE_STYLE_USAGE ( .BOTH. , #10006 ) ;
#13882 = CARTESIAN_POINT ( 'NONE',  ( 6.780834057763294634E-14, -6.250000000000000888, 10.49999999999998224 ) ) ;
#13883 = CARTESIAN_POINT ( 'NONE',  ( -2.500000000000000444, 186.0000000000000000, 7.000000000000000000 ) ) ;
#13884 = CARTESIAN_POINT ( 'NONE',  ( -1.885954199498669270, 228.0508284750123664, 6.386186391668034368 ) ) ;
#13885 = UNCERTAINTY_MEASURE_WITH_UNIT (LENGTH_MEASURE( 1.000000000000000082E-05 ), #13790, 'distance_accuracy_value', 'NONE');
#13886 = CYLINDRICAL_SURFACE ( 'NONE', #2713, 6.000000000000000888 ) ;
#13887 = B_SPLINE_CURVE_WITH_KNOTS ( 'NONE', 3,
 ( #3852, #8726, #5456, #15155, #11719, #10226, #1857, #10303, #6807, #15310, #822, #11643, #10380, #9267, #6731, #745, #510, #5687, #12600, #12912, #3058, #15077, #4250, #11563, #9120, #8964, #7909, #12752, #10534, #7834, #11409, #5380, #659, #1699, #5532, #15230, #4333, #7754, #1933, #3137, #9190, #13949 ),
 .UNSPECIFIED., .F., .F.,
 ( 4, 2, 2, 2, 2, 2, 2, 2, 2, 2, 2, 2, 2, 2, 2, 2, 2, 2, 2, 2, 4 ),
 ( 0.000000000000000000, 0.06250000000000002776, 0.1250000000000000555, 0.1562500000000000555, 0.1875000000000000833, 0.2500000000000001110, 0.3125000000000001110, 0.3750000000000001665, 0.4062500000000001665, 0.4375000000000001110, 0.5000000000000001110, 0.5625000000000000000, 0.5937500000000000000, 0.6250000000000000000, 0.6875000000000001110, 0.7500000000000001110, 0.8125000000000001110, 0.8437500000000001110, 0.8750000000000001110, 0.9375000000000001110, 1.000000000000000000 ),
 .UNSPECIFIED. ) ;
#13888 = CARTESIAN_POINT ( 'NONE',  ( -4.070051655338084551, -4.744673454622494901, 10.62632671364005077 ) ) ;
#13889 = CARTESIAN_POINT ( 'NONE',  ( -1.265664690411614835E-16, 2.066987299999999639, -1.349999998907525534 ) ) ;
#13890 = CARTESIAN_POINT ( 'NONE',  ( -5.454892180317694184E-16, 185.4000000000000057, 9.500000000000001776 ) ) ;
#13891 = FACE_OUTER_BOUND ( 'NONE', #2784, .T. ) ;
#13893 = VERTEX_POINT ( 'NONE', #1701 ) ;
#13892 = CARTESIAN_POINT ( 'NONE',  ( 0.8561741729129460632, 186.6999999989075150, 9.066987299999999195 ) ) ;
#13894 = CARTESIAN_POINT ( 'NONE',  ( -3.420659742068413944, -4.931142898501715166, 17.00004946353775992 ) ) ;
#13895 = CARTESIAN_POINT ( 'NONE',  ( 3.632753594129150887, 4.777047695051116705, 25.49995053646222232 ) ) ;
#13896 = EDGE_CURVE ( 'NONE', #9247, #1121, #3930, .T. ) ;
#13897 = AXIS2_PLACEMENT_3D ( 'NONE', #4859, #7245, #4777 ) ;
#13898 = CARTESIAN_POINT ( 'NONE',  ( -5.999999999999999112, 222.7460571280668091, 12.08513476933103448 ) ) ;
#13899 = CARTESIAN_POINT ( 'NONE',  ( -3.061616997868391523E-16, 189.0000000000000000, 7.000000000000000000 ) ) ;
#13900 = CARTESIAN_POINT ( 'NONE',  ( 2.208001381734123747, 188.9999999987420836, 8.182568187628087131 ) ) ;
#13901 = CARTESIAN_POINT ( 'NONE',  ( -5.558508435838157347, -2.857531096718993080, 11.49999999999998224 ) ) ;
#13902 = CARTESIAN_POINT ( 'NONE',  ( 6.123233995736766282E-16, 22.00000000000000000, 5.000000000000000000 ) ) ;
#13903 = DIRECTION ( 'NONE',  ( 0.9510565162951499785, 0.3090169943749582204, 0.000000000000000000 ) ) ;
#13904 = CARTESIAN_POINT ( 'NONE',  ( 6.172614129015267181, -0.9817721000786672203, 24.23763026556124700 ) ) ;
#13905 = CARTESIAN_POINT ( 'NONE',  ( -5.558508435838229289, 2.857531096718854524, 5.000000000000004441 ) ) ;
#13906 = LINE ( 'NONE', #14876, #5950 ) ;
#13907 = ORIENTED_EDGE ( 'NONE', *, *, #12935, .T. ) ;
#13908 = CARTESIAN_POINT ( 'NONE',  ( -1.461580736456473240, 186.1499999989075320, 5.538419263543526760 ) ) ;
#13909 = AXIS2_PLACEMENT_3D ( 'NONE', #5055, #7439, #5935 ) ;
#13910 = EDGE_LOOP ( 'NONE', ( #1991, #1604, #2184, #5360 ) ) ;
#13911 = CARTESIAN_POINT ( 'NONE',  ( -5.782947755040631854, 1.603807858344106441, 25.47398020122238549 ) ) ;
#13912 = AXIS2_PLACEMENT_3D ( 'NONE', #3412, #7089, #10741 ) ;
#13913 = ORIENTED_EDGE ( 'NONE', *, *, #9736, .F. ) ;
#13914 = CARTESIAN_POINT ( 'NONE',  ( -4.322356511625880415, 7.650514973136431252, 17.99999999999998934 ) ) ;
#13915 = CARTESIAN_POINT ( 'NONE',  ( -2.066987299999999195, -0.8561741729129466183, -2.699999998907525178 ) ) ;
#13916 = CARTESIAN_POINT ( 'NONE',  ( 0.000000000000000000, 184.0000000000000000, 7.000000000000000000 ) ) ;
#13917 = AXIS2_PLACEMENT_3D ( 'NONE', #767, #15334, #9288 ) ;
#13918 = EDGE_CURVE ( 'NONE', #8844, #5961, #13170, .T. ) ;
#13919 = CARTESIAN_POINT ( 'NONE',  ( 5.747343991580251554, -1.727858744772061916, 23.50007997643738022 ) ) ;
#13920 = CARTESIAN_POINT ( 'NONE',  ( -1.767766952966369098, 1.767766952966369098, -2.399999999999999911 ) ) ;
#13921 = CARTESIAN_POINT ( 'NONE',  ( -5.570722351696259622, -2.834100162821977520, 5.261902130840119263 ) ) ;
#13922 = CARTESIAN_POINT ( 'NONE',  ( -3.632151824461037570, -4.777505256984632354, 10.49995067926685977 ) ) ;
#13923 = FACE_OUTER_BOUND ( 'NONE', #15076, .T. ) ;
#13924 = CARTESIAN_POINT ( 'NONE',  ( 0.8561741729129451750, 2.066987299999999639, 1.200000001092474733 ) ) ;
#13925 = SHAPE_REPRESENTATION ( 'Rigid Mounting Base Clamp', ( #14201 ), #5333 ) ;
#13926 = CARTESIAN_POINT ( 'NONE',  ( 3.107278289587142694, 5.134157760522080061, 12.37364704684420857 ) ) ;
#13927 = EDGE_LOOP ( 'NONE', ( #15060, #6535, #5745, #7832 ) ) ;
#13928 = ORIENTED_EDGE ( 'NONE', *, *, #5208, .T. ) ;
#13929 = AXIS2_PLACEMENT_3D ( 'NONE', #899, #5768, #3365 ) ;
#13930 = VERTEX_POINT ( 'NONE', #13560 ) ;
#13931 = CARTESIAN_POINT ( 'NONE',  ( 2.668367453516524712, -5.373994336898185509, 24.63061695532138629 ) ) ;
#13932 = CARTESIAN_POINT ( 'NONE',  ( -5.385276659965230388E-16, 226.3251816629291966, 4.486670979098442480 ) ) ;
#13933 = ORIENTED_EDGE ( 'NONE', *, *, #13177, .F. ) ;
#13934 = CARTESIAN_POINT ( 'NONE',  ( 5.375886393124439167, -2.665038680141179395, 18.50439760644211518 ) ) ;
#13935 = CARTESIAN_POINT ( 'NONE',  ( 1.035533905932739085, -2.500000000000000000, -1.149999997815050357 ) ) ;
#13936 = EDGE_CURVE ( 'NONE', #3208, #3143, #7842, .T. ) ;
#13937 = CARTESIAN_POINT ( 'NONE',  ( -0.2619041840693476231, 6.245686665308508800, 17.02605849433793495 ) ) ;
#13938 = DIRECTION ( 'NONE',  ( -1.000000000000000000, 0.000000000000000000, 0.000000000000000000 ) ) ;
#13939 = CARTESIAN_POINT ( 'NONE',  ( 1.767766952966368432, 188.5999999978150470, 8.767766952966368876 ) ) ;
#13940 = CYLINDRICAL_SURFACE ( 'NONE', #4461, 1.000000000000000666 ) ;
#13941 = CARTESIAN_POINT ( 'NONE',  ( 5.665707375537479606, 1.979196487016660955, 19.00007961174475568 ) ) ;
#13942 = CARTESIAN_POINT ( 'NONE',  ( -1.361387964035781121E-13, 66.00000000000000000, 9.750000000000003553 ) ) ;
#13943 = AXIS2_PLACEMENT_3D ( 'NONE', #2753, #11183, #1391 ) ;
#13944 = AXIS2_PLACEMENT_3D ( 'NONE', #14297, #10500, #8035 ) ;
#13945 = CARTESIAN_POINT ( 'NONE',  ( -5.665308849928819335, -1.980336949702520721, 4.000079976437387330 ) ) ;
#13946 = CARTESIAN_POINT ( 'NONE',  ( -1.785671180686238868, 228.5485690224869586, 7.823689482036285447 ) ) ;
#13947 = CARTESIAN_POINT ( 'NONE',  ( 2.996417732210459484, 5.485687819086964900, 18.61396179408071561 ) ) ;
#13948 = ORIENTED_EDGE ( 'NONE', *, *, #1709, .F. ) ;
#13949 = CARTESIAN_POINT ( 'NONE',  ( 1.767766984964215471, 1.767766920968521616, -2.500000000000000444 ) ) ;
#13950 = VERTEX_POINT ( 'NONE', #7756 ) ;
#13951 = CARTESIAN_POINT ( 'NONE',  ( 2.817313151351187983, -5.579000502529432026, 5.000000000000004441 ) ) ;
#13952 = CARTESIAN_POINT ( 'NONE',  ( -2.500000000000000000, 0.000000000000000000, 2.500000000000000000 ) ) ;
#13953 = AXIS2_PLACEMENT_3D ( 'NONE', #8833, #13663, #9220 ) ;
#13954 = CARTESIAN_POINT ( 'NONE',  ( -7.180990026460726483, -3.384707322287581199, 11.49999999999998224 ) ) ;
#13955 = CARTESIAN_POINT ( 'NONE',  ( 5.858736126997189153, 2.179962889276912286, 23.52640428276698614 ) ) ;
#13956 = AXIS2_PLACEMENT_3D ( 'NONE', #8602, #2374, #1105 ) ;
#13957 = B_SPLINE_CURVE_WITH_KNOTS ( 'NONE', 3,
 ( #6188, #13410, #4912, #9769, #12058, #1083, #5944, #13090, #3465, #9604, #6025, #15648, #14443, #13330, #8417, #8501, #15571, #5864 ),
 .UNSPECIFIED., .F., .F.,
 ( 4, 2, 2, 2, 2, 2, 2, 2, 4 ),
 ( 0.000000000000000000, 0.0003914904498596249007, 0.0007829808997192496929, 0.001174471349578874377, 0.001565961799438498952, 0.001957452249298123528, 0.002348942699157748754, 0.002740433149017373546, 0.003131923598876997904 ),
 .UNSPECIFIED. ) ;
#13958 = DIRECTION ( 'NONE',  ( -6.123233995736766036E-17, 1.000000000000000000, 0.000000000000000000 ) ) ;
#13959 = CYLINDRICAL_SURFACE ( 'NONE', #2071, 2.499999999999999556 ) ;
#13960 = CARTESIAN_POINT ( 'NONE',  ( 6.176542424588124192, -0.9554180641285233699, 31.13063932754212360 ) ) ;
#13961 = CARTESIAN_POINT ( 'NONE',  ( 1.767766952966369320, -1.767766952966368654, -1.200000000000000178 ) ) ;
#13962 = CARTESIAN_POINT ( 'NONE',  ( -4.196288036172386882, -4.288789315524898171, 31.50312048902376105 ) ) ;
#13963 = CARTESIAN_POINT ( 'NONE',  ( -1.530808498934191571E-16, 2.500000000000000000, 1.600000002184949865 ) ) ;
#13964 = CARTESIAN_POINT ( 'NONE',  ( -2.500000000000000444, 185.0999999978150754, 7.000000000000000000 ) ) ;
#13965 = EDGE_CURVE ( 'NONE', #8394, #11747, #12018, .T. ) ;
#13967 = CARTESIAN_POINT ( 'NONE',  ( 1.692341931978252223, 227.9167330860961442, 5.998911260178718230 ) ) ;
#13966 = PRESENTATION_LAYER_ASSIGNMENT (  '', '', ( #9157 ) ) ;
#13968 = FACE_BOUND ( 'NONE', #10535, .T. ) ;
#13969 = CARTESIAN_POINT ( 'NONE',  ( 6.155973317223295105, -1.081218830693672972, 30.49691356133954301 ) ) ;
#13970 = EDGE_CURVE ( 'NONE', #13435, #1133, #15466, .T. ) ;
#13971 = B_SPLINE_CURVE_WITH_KNOTS ( 'NONE', 3,
 ( #15395, #9344, #14185, #5461, #8155, #2414, #4652, #983, #1063, #15712, #14589, #13151, #10692, #5927, #10930, #3444, #8484, #9504 ),
 .UNSPECIFIED., .F., .F.,
 ( 4, 2, 2, 2, 2, 2, 2, 2, 4 ),
 ( 0.000000000000000000, 0.0003914898357794971157, 0.0007829796715589942314, 0.001174469507338491347, 0.001565959343117987379, 0.001957449178897484061, 0.002348939014676979659, 0.002740428850456476124, 0.003131918686235972155 ),
 .UNSPECIFIED. ) ;
#13972 = CARTESIAN_POINT ( 'NONE',  ( 0.8561741729129465073, -2.066987299999999195, -0.09999999890752520049 ) ) ;
#13973 = CARTESIAN_POINT ( 'NONE',  ( -1.050320854595332420E-16, 188.2000000000000171, 4.500000000000000000 ) ) ;
#13974 = CARTESIAN_POINT ( 'NONE',  ( -2.817313151351372724, 5.579000502529338767, 24.49999999999999289 ) ) ;
#13975 = EDGE_CURVE ( 'NONE', #2054, #11100, #8866, .T. ) ;
#13977 = VERTEX_POINT ( 'NONE', #203 ) ;
#13976 = CARTESIAN_POINT ( 'NONE',  ( -0.1306171417086578468, -6.000000000000006217, 23.50000000000000000 ) ) ;
#13978 = FACE_OUTER_BOUND ( 'NONE', #7559, .T. ) ;
#13979 = CARTESIAN_POINT ( 'NONE',  ( 5.487097279078491319, -2.429065649168680174, 17.20047945897285047 ) ) ;
#13980 = CARTESIAN_POINT ( 'NONE',  ( 2.283493650000000486, 184.1249999994537632, 7.000000000000000000 ) ) ;
#13981 =( NAMED_UNIT ( * ) PLANE_ANGLE_UNIT ( ) SI_UNIT ( $, .RADIAN. ) );
#13982 = CARTESIAN_POINT ( 'NONE',  ( 2.832543757336219326, 189.3479566575481385, 6.034102192250282215 ) ) ;
#13983 = LINE ( 'NONE', #11439, #7065 ) ;
#13984 = DIRECTION ( 'NONE',  ( -0.5877852522924685852, -0.8090169943749508930, 0.000000000000000000 ) ) ;
#13985 = CARTESIAN_POINT ( 'NONE',  ( 0.9660064634511277282, 228.8301302322938966, 8.636854315157751927 ) ) ;
#13986 = CARTESIAN_POINT ( 'NONE',  ( 5.616116467183726257, -2.743044348085402540, 23.99574050496988065 ) ) ;
#13987 = CARTESIAN_POINT ( 'NONE',  ( 0.02292651764862485564, 0.4000000000000062395, 2.515500884275507776 ) ) ;
#13988 = DIRECTION ( 'NONE',  ( -0.5877852522924685852, -0.8090169943749508930, 0.000000000000000000 ) ) ;
#13989 = ORIENTED_EDGE ( 'NONE', *, *, #10999, .F. ) ;
#13990 = CARTESIAN_POINT ( 'NONE',  ( -2.066760391300492827E-16, 189.4499999989075150, 4.933012699999999029 ) ) ;
#13991 = AXIS2_PLACEMENT_3D ( 'NONE', #4434, #9368, #8256 ) ;
#13992 = CARTESIAN_POINT ( 'NONE',  ( -9.750000000000003553, 184.0000000000000000, -3.401296724241641415E-14 ) ) ;
#13993 = VERTEX_POINT ( 'NONE', #2670 ) ;
#13994 = DIRECTION ( 'NONE',  ( 0.000000000000000000, 1.000000000000000000, 0.000000000000000000 ) ) ;
#13995 = DIRECTION ( 'NONE',  ( 0.000000000000000000, 0.000000000000000000, 1.000000000000000000 ) ) ;
#13996 = CARTESIAN_POINT ( 'NONE',  ( 5.531796221294892568, 2.326749136277177499, 17.12621569129737509 ) ) ;
#13997 = CARTESIAN_POINT ( 'NONE',  ( -2.066987300000000971, 184.6999999989075150, 7.856174172912944620 ) ) ;
#13998 = CARTESIAN_POINT ( 'NONE',  ( -0.1306394121197269609, 6.250000000000005329, 23.49999999999999289 ) ) ;
#13999 = EDGE_CURVE ( 'NONE', #3420, #1004, #5814, .T. ) ;
#14000 = CARTESIAN_POINT ( 'NONE',  ( -1.530808498934191571E-16, 2.500000000000000000, -2.500000000000000000 ) ) ;
#14001 = DIRECTION ( 'NONE',  ( -0.000000000000000000, 1.000000000000000000, -0.000000000000000000 ) ) ;
#14002 = CARTESIAN_POINT ( 'NONE',  ( 3.659182332138577465E-16, 215.0542865858234336, 7.296348638359030581 ) ) ;
#14003 = CYLINDRICAL_SURFACE ( 'NONE', #15369, 1.000000000000000666 ) ;
#14004 = CARTESIAN_POINT ( 'NONE',  ( 4.416779112813637553, 4.422345839825811531, 31.26225281721713856 ) ) ;
#14005 = CARTESIAN_POINT ( 'NONE',  ( -0.6829126361173057935, 228.2303005364134094, 10.09526665386122346 ) ) ;
#14006 = EDGE_LOOP ( 'NONE', ( #8791, #10928, #14586, #6925 ) ) ;
#14007 = EDGE_CURVE ( 'NONE', #159, #15355, #6344, .T. ) ;
#14008 = EDGE_LOOP ( 'NONE', ( #4726, #570 ) ) ;
#14009 = ORIENTED_EDGE ( 'NONE', *, *, #1670, .F. ) ;
#14010 = AXIS2_PLACEMENT_3D ( 'NONE', #7434, #9675, #1145 ) ;
#14011 = CARTESIAN_POINT ( 'NONE',  ( 2.668367453516524268, -5.373994336898184621, 24.49999999999999289 ) ) ;
#14012 = DIRECTION ( 'NONE',  ( 0.000000000000000000, 0.000000000000000000, 1.000000000000000000 ) ) ;
#14013 = B_SPLINE_CURVE_WITH_KNOTS ( 'NONE', 3,
 ( #8081, #7546, #5389, #15087, #7845, #9129, #9431, #4580, #13075, #2175, #11964, #1224, #8160, #5775, #5932, #1146, #7287, #5854 ),
 .UNSPECIFIED., .F., .F.,
 ( 4, 2, 2, 2, 2, 2, 2, 2, 4 ),
 ( 0.003131486019301977283, 0.003522824630466687024, 0.003914163241631397200, 0.004305501852796106074, 0.004696840463960814949, 0.005088179075125523823, 0.005479517686290232698, 0.005870856297454941572, 0.006262194908619650446 ),
 .UNSPECIFIED. ) ;
#14014 = ORIENTED_EDGE ( 'NONE', *, *, #5939, .T. ) ;
#14015 = CARTESIAN_POINT ( 'NONE',  ( 5.620786884546348006, -2.102685372472733683, 18.97358595436693207 ) ) ;
#14016 = PRODUCT_DEFINITION_SHAPE ( 'NONE', 'NONE',  #15751 ) ;
#14017 = CARTESIAN_POINT ( 'NONE',  ( 1.767766952966368654, 1.767766952966369098, 1.500000002184949777 ) ) ;
#14018 = CARTESIAN_POINT ( 'NONE',  ( -4.070051655338123631, 4.744673454622464703, 31.87367328635992791 ) ) ;
#14019 = CARTESIAN_POINT ( 'NONE',  ( 0.000000000000000000, 0.000000000000000000, 0.000000000000000000 ) ) ;
#14020 = CARTESIAN_POINT ( 'NONE',  ( -0.8561741729129452860, 184.6999999989075150, 4.933012699999999029 ) ) ;
#14021 = CARTESIAN_POINT ( 'NONE',  ( 1.767766952966369320, -1.767766952966368654, 2.006999999978150484 ) ) ;
#14022 = CARTESIAN_POINT ( 'NONE',  ( -4.152999119458083754, 4.671604476854259502, 18.80026515017675237 ) ) ;
#14023 = PRODUCT_CONTEXT ( 'NONE', #9645, 'mechanical' ) ;
#14024 = CARTESIAN_POINT ( 'NONE',  ( -1.524659305057740610E-16, 189.0000000000000000, 4.500000000000000000 ) ) ;
#14025 = VECTOR ( 'NONE', #5659, 1000.000000000000000 ) ;
#14026 = CARTESIAN_POINT ( 'NONE',  ( -2.500000000000000444, 189.1199999975965795, 5.964466094067261359 ) ) ;
#14027 = CARTESIAN_POINT ( 'NONE',  ( 2.050915569729614862, 227.9948459642048419, 9.402920486592190485 ) ) ;
#14028 = CARTESIAN_POINT ( 'NONE',  ( -8.666684749742561339E-31, 189.0000000000000000, -9.500000000000000000 ) ) ;
#14029 = ORIENTED_EDGE ( 'NONE', *, *, #12828, .T. ) ;
#14030 = EDGE_LOOP ( 'NONE', ( #1526, #1761, #12734, #3021 ) ) ;
#14031 = CARTESIAN_POINT ( 'NONE',  ( 4.435347140101073116, -4.403429997944471985, 5.132341256341692137 ) ) ;
#14032 = CARTESIAN_POINT ( 'NONE',  ( -1.768703179866833342, 189.0000639513403939, 5.233169770031948609 ) ) ;
#14033 = FACE_BOUND ( 'NONE', #894, .T. ) ;
#14035 = ORIENTED_EDGE ( 'NONE', *, *, #14369, .T. ) ;
#14034 = CIRCLE ( 'NONE', #5421, 3.000000000000000888 ) ;
#14036 = CARTESIAN_POINT ( 'NONE',  ( 4.153440676704393653, 4.671190581744498083, 10.70045537531157365 ) ) ;
#14037 = FACE_BOUND ( 'NONE', #8499, .T. ) ;
#14038 = CARTESIAN_POINT ( 'NONE',  ( 3.254737477227961584, -5.337033878705229384, 17.12632671364005077 ) ) ;
#14039 = CARTESIAN_POINT ( 'NONE',  ( -2.500000000000000444, 1.035533905932737753, -1.549999999999999600 ) ) ;
#14040 = DIRECTION ( 'NONE',  ( -6.123233995736766036E-17, 1.000000000000000000, 0.000000000000000000 ) ) ;
#14041 = CARTESIAN_POINT ( 'NONE',  ( 1.767766952966368654, 1.767766952966369098, 1.500000002184949777 ) ) ;
#14042 = CARTESIAN_POINT ( 'NONE',  ( 0.000000000000000000, 186.4999999978150527, 4.500000000000000000 ) ) ;
#14043 = CARTESIAN_POINT ( 'NONE',  ( -1.939606487604890850, 228.4085856529902117, 7.419409526801750587 ) ) ;
#14044 = FACE_BOUND ( 'NONE', #6653, .T. ) ;
#14045 = CARTESIAN_POINT ( 'NONE',  ( 0.5030929395822668626, 6.230885867001124900, 23.62600319116549841 ) ) ;
#14046 = CARTESIAN_POINT ( 'NONE',  ( 1.461580736456473018, -1.461580736456472573, -0.8499999989075254225 ) ) ;
#14047 = CARTESIAN_POINT ( 'NONE',  ( -2.500000000000000444, 186.7500000000000000, 5.964466094067261359 ) ) ;
#14048 = CARTESIAN_POINT ( 'NONE',  ( -4.435347140101220553, 4.403429997944323659, 24.63063932754212360 ) ) ;
#14050 = ORIENTED_EDGE ( 'NONE', *, *, #3366, .T. ) ;
#14049 = CARTESIAN_POINT ( 'NONE',  ( -1.000079958707936756, -5.916066267613731888, 24.63152738882033432 ) ) ;
#14051 = DIRECTION ( 'NONE',  ( 0.000000000000000000, 0.000000000000000000, 1.000000000000000000 ) ) ;
#14052 = ADVANCED_FACE ( 'NONE', ( #15312 ), #4335, .F. ) ;
#14053 = CARTESIAN_POINT ( 'NONE',  ( -5.915653884842686061, 1.003805156977559676, 23.99560239355785640 ) ) ;
#14054 = CARTESIAN_POINT ( 'NONE',  ( -2.917684139655223330, 189.8446451309251302, 8.046806756071347877 ) ) ;
#14055 =( LENGTH_UNIT ( ) NAMED_UNIT ( * ) SI_UNIT ( .MILLI., .METRE. ) );
#14056 = DIRECTION ( 'NONE',  ( 0.5877852522924802425, -0.8090169943749422332, 0.000000000000000000 ) ) ;
#14057 = CARTESIAN_POINT ( 'NONE',  ( -0.5227993896667307849, 227.6261285884132235, 5.159628895875891352 ) ) ;
#14058 = CARTESIAN_POINT ( 'NONE',  ( 0.2588337889006175341, 228.9066910274044346, 8.857966258178848307 ) ) ;
#14059 = CARTESIAN_POINT ( 'NONE',  ( 6.172651332693092741, 0.9815532474593937629, 11.23809786915985853 ) ) ;
#14060 = EDGE_CURVE ( 'NONE', #11314, #11875, #1786, .T. ) ;
#14061 = CARTESIAN_POINT ( 'NONE',  ( 0.002345414276150574722, 0.4000000000000027978, 2.475568618642806307 ) ) ;
#14062 = DIRECTION ( 'NONE',  ( -1.000000000000000000, 0.000000000000000000, 0.000000000000000000 ) ) ;
#14063 = ORIENTED_EDGE ( 'NONE', *, *, #6146, .F. ) ;
#14064 = CARTESIAN_POINT ( 'NONE',  ( 0.8561741729129457301, 185.1999999989075150, 4.933012699999999029 ) ) ;
#14065 = CARTESIAN_POINT ( 'NONE',  ( -0.9735856429312097493, 5.920699391845040793, 11.76285283906727841 ) ) ;
#14066 = EDGE_LOOP ( 'NONE', ( #11977, #10539, #2555, #13596 ) ) ;
#14067 = DIRECTION ( 'NONE',  ( 0.000000000000000000, 0.000000000000000000, 1.000000000000000000 ) ) ;
#14068 = EDGE_CURVE ( 'NONE', #13757, #3740, #5578, .T. ) ;
#14069 = CARTESIAN_POINT ( 'NONE',  ( -3.107583187530343682, -5.133966411712735933, 5.873806827147109111 ) ) ;
#14070 = CARTESIAN_POINT ( 'NONE',  ( 7.490007020835692586, -2.433650805992223720, 31.00000000000000000 ) ) ;
#14071 = FACE_OUTER_BOUND ( 'NONE', #4230, .T. ) ;
#14072 =( LENGTH_UNIT ( ) NAMED_UNIT ( * ) SI_UNIT ( .MILLI., .METRE. ) );
#14073 = CARTESIAN_POINT ( 'NONE',  ( -3.255013540813561423, -5.336859797930882721, 5.873819640450717472 ) ) ;
#14074 = CARTESIAN_POINT ( 'NONE',  ( 4.592425496802573972E-16, -2.500000000000000000, 0.4000000021849499099 ) ) ;
#14075 = CARTESIAN_POINT ( 'NONE',  ( -5.558508435838189321, -2.857531096718932684, 4.869393092765017528 ) ) ;
#14076 = CARTESIAN_POINT ( 'NONE',  ( 5.999999999999999112, 186.5669965222008670, 9.317226423031115701 ) ) ;
#14077 = CARTESIAN_POINT ( 'NONE',  ( -5.558508435838096950, -2.857531096719117425, 24.63063932754212715 ) ) ;
#14078 = CARTESIAN_POINT ( 'NONE',  ( -5.935543223013826974, -0.8771126767608833363, 17.86763921416087442 ) ) ;
#14079 = DIRECTION ( 'NONE',  ( 6.123233995736766036E-17, -1.000000000000000000, -0.000000000000000000 ) ) ;
#14080 = CIRCLE ( 'NONE', #3672, 3.000000000000000888 ) ;
#14081 = VERTEX_POINT ( 'NONE', #11566 ) ;
#14082 = EDGE_LOOP ( 'NONE', ( #5120, #1291 ) ) ;
#14083 = ORIENTED_EDGE ( 'NONE', *, *, #5221, .F. ) ;
#14084 = CARTESIAN_POINT ( 'NONE',  ( 3.633127580202175189, -4.776802569231135109, 25.50007961174476634 ) ) ;
#14085 = CARTESIAN_POINT ( 'NONE',  ( 3.659182332138577465E-16, 202.3580807015429457, 7.308726713069390257 ) ) ;
#14086 = VERTEX_POINT ( 'NONE', #661 ) ;
#14087 = CARTESIAN_POINT ( 'NONE',  ( 1.035533905932737975, 184.9499999999999886, 4.500000000000001776 ) ) ;
#14088 = CARTESIAN_POINT ( 'NONE',  ( 1.767766952966368654, 1.767766952966369098, 0.7000000021849496212 ) ) ;
#14089 = VECTOR ( 'NONE', #6142, 1000.000000000000000 ) ;
#14090 = CARTESIAN_POINT ( 'NONE',  ( 6.021135683317711873, 1.680226122398159161, 18.97377282875267213 ) ) ;
#14091 = CARTESIAN_POINT ( 'NONE',  ( 1.353717517954364224E-13, 6.000000000000000888, 18.99999999999998934 ) ) ;
#14092 = CARTESIAN_POINT ( 'NONE',  ( -2.066987300000000083, 185.5999999989075775, 6.143825827087054492 ) ) ;
#14093 = EDGE_CURVE ( 'NONE', #13172, #4668, #5535, .T. ) ;
#14094 = CARTESIAN_POINT ( 'NONE',  ( -2.500000000000000000, 0.000000000000000000, 2.506999999978150484 ) ) ;
#14095 = B_SPLINE_CURVE_WITH_KNOTS ( 'NONE', 3,
 ( #10021, #1414, #11130, #1183, #5093, #4939, #3881, #9791, #14640, #1341, #9944, #7548, #6055, #12395, #1494, #6372, #11206, #4860 ),
 .UNSPECIFIED., .F., .F.,
 ( 4, 2, 2, 2, 2, 2, 2, 2, 4 ),
 ( 0.003131490185286089217, 0.003522829482338690147, 0.003914168779391291077, 0.004305508076443891573, 0.004696847373496492069, 0.005088186670549092565, 0.005479525967601693928, 0.005870865264654294424, 0.006262204561706894920 ),
 .UNSPECIFIED. ) ;
#14096 = APPLICATION_PROTOCOL_DEFINITION ( 'draft international standard', 'automotive_design', 1998, #7502 ) ;
#14097 = CARTESIAN_POINT ( 'NONE',  ( -2.066987299999999639, 0.000000000000000000, 2.050000001092474822 ) ) ;
#14098 = CARTESIAN_POINT ( 'NONE',  ( 1.767766952966368432, 188.6699999975965341, 8.767766952966368876 ) ) ;
#14099 = CARTESIAN_POINT ( 'NONE',  ( 0.3927937339364459546, 226.3329534510998542, 4.509583726312986762 ) ) ;
#14100 = EDGE_CURVE ( 'NONE', #4730, #11432, #11833, .T. ) ;
#14101 = CARTESIAN_POINT ( 'NONE',  ( -2.500000000000000444, 186.0000000000000000, 7.000000000000000000 ) ) ;
#14102 = ORIENTED_EDGE ( 'NONE', *, *, #7851, .T. ) ;
#14103 = CARTESIAN_POINT ( 'NONE',  ( -2.500000000000000000, -1.035533905932739307, 0.2500000021849497212 ) ) ;
#14104 = AXIS2_PLACEMENT_3D ( 'NONE', #8646, #1540, #14679 ) ;
#14105 = ORIENTED_EDGE ( 'NONE', *, *, #15274, .F. ) ;
#14106 = CARTESIAN_POINT ( 'NONE',  ( 2.817313151351188871, -5.579000502529433803, 5.130606907234995795 ) ) ;
#14107 =( REPRESENTATION_RELATIONSHIP ('NONE','NONE', #11191, #4596 ) REPRESENTATION_RELATIONSHIP_WITH_TRANSFORMATION ( #13461 )SHAPE_REPRESENTATION_RELATIONSHIP( ) );
#14108 = CARTESIAN_POINT ( 'NONE',  ( 7.490007020835728113, -2.433650805992114918, 17.99999999999998934 ) ) ;
#14109 = CARTESIAN_POINT ( 'NONE',  ( 6.020822430078827558, 1.681351817312285668, 23.52591457665828756 ) ) ;
#14110 = VERTEX_POINT ( 'NONE', #3683 ) ;
#14111 = CARTESIAN_POINT ( 'NONE',  ( 3.780072143464171752, 4.979057943639783268, 10.49991780678442410 ) ) ;
#14112 = DIRECTION ( 'NONE',  ( -1.000000000000000000, 0.000000000000000000, 0.000000000000000000 ) ) ;
#14113 = CARTESIAN_POINT ( 'NONE',  ( -1.767766952966368432, -1.767766952966369320, 1.800000000000000044 ) ) ;
#14114 = CIRCLE ( 'NONE', #9053, 1.999999999999999556 ) ;
#14115 = CARTESIAN_POINT ( 'NONE',  ( 2.500000000000000444, -1.035533905932737309, -1.150000000000000133 ) ) ;
#14116 = CARTESIAN_POINT ( 'NONE',  ( -4.435347140101154828, -4.403429997944389385, 24.63060690723497714 ) ) ;
#14117 = LINE ( 'NONE', #3377, #2919 ) ;
#14118 = CARTESIAN_POINT ( 'NONE',  ( -5.387129544537350156E-16, 185.2999999978150356, 9.500000000000001776 ) ) ;
#14119 = CARTESIAN_POINT ( 'NONE',  ( -1.984331290054332841, 228.3135221411288285, 7.144860682478253011 ) ) ;
#14120 = DIRECTION ( 'NONE',  ( -0.9510565162951544194, 0.3090169943749447312, 0.000000000000000000 ) ) ;
#14121 = CARTESIAN_POINT ( 'NONE',  ( -5.486741141153758328, 2.429871531109806249, 18.79888242247939800 ) ) ;
#14122 = CARTESIAN_POINT ( 'NONE',  ( -0.8561741729129455081, 2.066987299999999639, -2.899999998907526244 ) ) ;
#14123 = CARTESIAN_POINT ( 'NONE',  ( -5.929230630780102373E-16, 186.2000000000000171, 9.500000000000001776 ) ) ;
#14124 = CARTESIAN_POINT ( 'NONE',  ( 3.780072143464118906, -4.979057943639823236, 25.50008219321556879 ) ) ;
#14125 = AXIS2_PLACEMENT_3D ( 'NONE', #9475, #798, #12964 ) ;
#14127 = ORIENTED_EDGE ( 'NONE', *, *, #14600, .F. ) ;
#14126 = DIRECTION ( 'NONE',  ( 0.000000000000000000, 0.000000000000000000, 1.000000000000000000 ) ) ;
#14128 = DIRECTION ( 'NONE',  ( 0.5877852522924802425, -0.8090169943749422332, 0.000000000000000000 ) ) ;
#14129 = EDGE_CURVE ( 'NONE', #260, #10533, #11391, .T. ) ;
#14130 = CARTESIAN_POINT ( 'NONE',  ( -1.035533905932737975, 186.6500000000000057, 4.500000000000001776 ) ) ;
#14131 = CARTESIAN_POINT ( 'NONE',  ( -2.761685261155654381, 227.6665753604594045, 8.437282647672972757 ) ) ;
#14132 = FILL_AREA_STYLE_COLOUR ( '', #14982 ) ;
#14133 = CARTESIAN_POINT ( 'NONE',  ( 1.155845512882874626, 189.4310859332073562, 4.210941953806538685 ) ) ;
#14134 = CARTESIAN_POINT ( 'NONE',  ( -1.035533905932739529, 185.2800000002184504, 9.500000000000003553 ) ) ;
#14135 = FACE_OUTER_BOUND ( 'NONE', #9957, .T. ) ;
#14136 = AXIS2_PLACEMENT_3D ( 'NONE', #13248, #12053, #1152 ) ;
#14137 = CARTESIAN_POINT ( 'NONE',  ( 0.1297182620452491941, 228.9108343529357228, 8.869932418632497928 ) ) ;
#14138 = DIRECTION ( 'NONE',  ( -1.000000000000000000, 0.000000000000000000, 0.000000000000000000 ) ) ;
#14139 = CARTESIAN_POINT ( 'NONE',  ( 1.979652835806277785E-15, -0.001000000000000132727, 11.50000000000000000 ) ) ;
#14140 = CARTESIAN_POINT ( 'NONE',  ( -3.632151824461010925, -4.777505256984653670, 29.99995067926689174 ) ) ;
#14141 = ORIENTED_EDGE ( 'NONE', *, *, #8685, .F. ) ;
#14142 = CARTESIAN_POINT ( 'NONE',  ( -1.461580736456473018, 184.5499999989075093, 5.538419263543526760 ) ) ;
#14143 = EDGE_CURVE ( 'NONE', #12751, #15454, #14706, .T. ) ;
#14144 = DIRECTION ( 'NONE',  ( 0.000000000000000000, 0.000000000000000000, 1.000000000000000000 ) ) ;
#14145 = ORIENTED_EDGE ( 'NONE', *, *, #6110, .F. ) ;
#14146 = CARTESIAN_POINT ( 'NONE',  ( -1.767766952966369765, 186.0999999999999943, 8.767766952966368876 ) ) ;
#14147 = CIRCLE ( 'NONE', #9331, 2.750000000000002665 ) ;
#14148 = B_SPLINE_CURVE_WITH_KNOTS ( 'NONE', 3,
 ( #9218, #3162, #401, #5271, #4438, #8774, #690, #4062, #1515, #11225, #9963, #8932, #7491, #2638, #1434, #8019, #10041, #12857, #6838, #6311, #250, #5110, #14814, #15578, #4838, #11749, #9371, #3555, #5873, #15416, #14131, #15655, #8181, #13179, #4678, #12066, #3237, #1090, #11818, #9450, #6990, #10720, #1010, #2040, #14282, #5793, #10796, #8102, #3391, #9531, #11984, #4598, #851, #14452, #925, #4757, #2360, #8259, #10639, #4515, #15501, #13097, #7067, #2194, #11902, #14366, #3472, #8341, #5717, #6915, #1164, #2278, #7148, #12940, #5952, #9614, #8424, #13018, #13261, #7228, #6033, #10879 ),
 .UNSPECIFIED., .F., .F.,
 ( 4, 2, 2, 2, 2, 2, 2, 2, 1, 1, 2, 2, 2, 2, 2, 1, 1, 2, 2, 2, 2, 2, 1, 2, 2, 2, 2, 2, 1, 1, 1, 2, 2, 2, 2, 1, 1, 1, 2, 2, 2, 2, 1, 2, 2, 2, 4 ),
 ( 0.000000000000000000, 0.03125000000001913053, 0.04687500000002882417, 0.05468750000003370221, 0.05859375000003642919, 0.06250000000003916312, 0.09375000000006236678, 0.1093750000000735939, 0.1171875000000792005, 0.1210937500000814487, 0.1230468750000829475, 0.1250000000000844602, 0.1562500000001039724, 0.1718750000001137423, 0.1796875000001185163, 0.1835937500001208755, 0.1855468750001219302, 0.1865234375001218747, 0.1875000000001218192, 0.2187500000001719458, 0.2343750000001968703, 0.2421875000002100264, 0.2460937500002166600, 0.2480468750002199629, 0.2500000000002232659, 0.2812500000002847722, 0.2968750000003155254, 0.3046875000003299583, 0.3085937500003371192, 0.3105468750003417822, 0.3115234375003440581, 0.3120117187503441136, 0.3125000000003441136, 0.3437500000002909895, 0.3593750000002637890, 0.3671875000002502998, 0.3710937500002434719, 0.3730468750002405853, 0.3740234375002385314, 0.3750000000002364775, 0.4062500000001775247, 0.4218750000001476597, 0.4296875000001331157, 0.4335937500001255107, 0.4375000000001179057, 0.4687500000000588973, 0.5000000000000000000 ),
 .UNSPECIFIED. ) ;
#14149 = CARTESIAN_POINT ( 'NONE',  ( 1.461580736456472573, 185.1499999989075320, 8.461580736456474128 ) ) ;
#14150 = LINE ( 'NONE', #12875, #13405 ) ;
#14151 = CARTESIAN_POINT ( 'NONE',  ( -2.066987300000000527, 187.0499999989075093, 7.000000000000000000 ) ) ;
#14152 = CARTESIAN_POINT ( 'NONE',  ( -4.290821322214329214, -4.545321419741597424, 5.614419472454843962 ) ) ;
#14153 = CARTESIAN_POINT ( 'NONE',  ( 2.500000000000000444, -1.035533905932737309, 0.5500000021849498211 ) ) ;
#14154 = CARTESIAN_POINT ( 'NONE',  ( 2.449293598294706513E-15, 2.000000000000000000, 20.00000000000000000 ) ) ;
#14155 = CARTESIAN_POINT ( 'NONE',  ( 5.999999999999999112, 227.2817795252328210, 4.165129161027028459 ) ) ;
#14156 = ORIENTED_EDGE ( 'NONE', *, *, #10754, .F. ) ;
#14157 = CARTESIAN_POINT ( 'NONE',  ( 4.069684453406294367, 4.744965295353559043, 31.87380055247396271 ) ) ;
#14158 = CARTESIAN_POINT ( 'NONE',  ( -0.9737778612004134304, -5.920671847850539571, 17.73736375884649519 ) ) ;
#14159 = CIRCLE ( 'NONE', #2484, 4.000000000000001776 ) ;
#14160 = EDGE_CURVE ( 'NONE', #1022, #8273, #2351, .T. ) ;
#14161 = ORIENTED_EDGE ( 'NONE', *, *, #12092, .F. ) ;
#14162 = ORIENTED_EDGE ( 'NONE', *, *, #10606, .T. ) ;
#14163 = EDGE_LOOP ( 'NONE', ( #14162, #6554, #6185, #7778 ) ) ;
#14164 = CARTESIAN_POINT ( 'NONE',  ( -5.984759433606990697, -1.806271833852358011, 10.49991780678442232 ) ) ;
#14165 = CARTESIAN_POINT ( 'NONE',  ( -3.420659742068434817, 4.931142898501699179, 12.49995053646221166 ) ) ;
#14166 = ORIENTED_EDGE ( 'NONE', *, *, #11861, .F. ) ;
#14167 = AXIS2_PLACEMENT_3D ( 'NONE', #12384, #6442, #6518 ) ;
#14168 = CARTESIAN_POINT ( 'NONE',  ( -1.035533905932737753, 2.500000000000000444, 0.8500000021849496434 ) ) ;
#14169 = VECTOR ( 'NONE', #13515, 1000.000000000000000 ) ;
#14170 = CARTESIAN_POINT ( 'NONE',  ( -5.408775798201155283, -2.598833957129672800, 31.61397738943081492 ) ) ;
#14171 = CARTESIAN_POINT ( 'NONE',  ( -2.931156713028388427, -5.520271803279265477, 4.495630303198470124 ) ) ;
#14172 = CARTESIAN_POINT ( 'NONE',  ( -2.500000000000000888, 188.3499999978150186, 8.035533905932737753 ) ) ;
#14173 = CARTESIAN_POINT ( 'NONE',  ( 2.500000000000000444, -1.035533905932737309, -1.943000000021849472 ) ) ;
#14174 = CARTESIAN_POINT ( 'NONE',  ( -1.035533905932737753, 185.7499999978150527, 4.500000000000001776 ) ) ;
#14175 = CARTESIAN_POINT ( 'NONE',  ( -1.461580736456472351, -1.461580736456473018, -0.2499999989075251672 ) ) ;
#14176 = CARTESIAN_POINT ( 'NONE',  ( -1.767766952966369320, 189.0699999975965397, 5.232233047033630235 ) ) ;
#14177 = CARTESIAN_POINT ( 'NONE',  ( 2.998835045281009304, 227.2583357984985639, 7.235791215503737384 ) ) ;
#14178 = CARTESIAN_POINT ( 'NONE',  ( -1.035533905932737753, 2.500000000000000444, 0.8500000021849498655 ) ) ;
#14179 = AXIS2_PLACEMENT_3D ( 'NONE', #10612, #4812, #6003 ) ;
#14180 = VERTEX_POINT ( 'NONE', #29 ) ;
#14181 = CARTESIAN_POINT ( 'NONE',  ( 2.500000000000000000, 188.6999999978150697, 7.000000000000000000 ) ) ;
#14182 = EDGE_CURVE ( 'NONE', #11235, #3287, #3254, .T. ) ;
#14183 = EDGE_LOOP ( 'NONE', ( #7260, #3315, #14899, #14276 ) ) ;
#14184 = CARTESIAN_POINT ( 'NONE',  ( -0.8738043859790136647, 6.188821459035888317, 12.00341560223746207 ) ) ;
#14185 = CARTESIAN_POINT ( 'NONE',  ( 4.267936573529204303, -4.217499624512243805, 17.73770962164069331 ) ) ;
#14186 = FACE_BOUND ( 'NONE', #1840, .T. ) ;
#14187 = VERTEX_POINT ( 'NONE', #3992 ) ;
#14188 = CARTESIAN_POINT ( 'NONE',  ( -5.931817299736841242, 0.9033986943602623221, 17.73770962164069331 ) ) ;
#14189 = EDGE_CURVE ( 'NONE', #9498, #14110, #7337, .T. ) ;
#14190 = AXIS2_PLACEMENT_3D ( 'NONE', #704, #6694, #5576 ) ;
#14191 = CARTESIAN_POINT ( 'NONE',  ( 0.000000000000000000, 0.000000000000000000, 53.67766952966368876 ) ) ;
#14192 = CARTESIAN_POINT ( 'NONE',  ( -3.158825713737595020, 5.393784879207108141, 12.29933148907576346 ) ) ;
#14193 = CARTESIAN_POINT ( 'NONE',  ( 4.592425496802573972E-16, -2.500000000000000000, -2.100000000000000089 ) ) ;
#14194 = CARTESIAN_POINT ( 'NONE',  ( 1.354942164390165777E-13, -6.250000000000000888, 16.99999999999998579 ) ) ;
#14195 = CARTESIAN_POINT ( 'NONE',  ( 0.08922814936599068880, 0.4000000000000062395, -2.551651095287820414 ) ) ;
#14196 = CARTESIAN_POINT ( 'NONE',  ( 1.767766952966369320, 185.5999999978150754, 5.232233047033630235 ) ) ;
#14197 = CARTESIAN_POINT ( 'NONE',  ( -1.826974499845722466, 228.5193582813216153, 7.739327195479140720 ) ) ;
#14198 = DIRECTION ( 'NONE',  ( -0.000000000000000000, 1.000000000000000000, -0.000000000000000000 ) ) ;
#14199 = DIRECTION ( 'NONE',  ( 0.000000000000000000, 1.000000000000000000, 0.000000000000000000 ) ) ;
#14200 = CARTESIAN_POINT ( 'NONE',  ( 1.461580736456472573, 1.461580736456472795, -2.249999998907525001 ) ) ;
#14201 = AXIS2_PLACEMENT_3D ( 'NONE', #6680, #11513, #1651 ) ;
#14202 = EDGE_CURVE ( 'NONE', #14655, #1178, #183, .T. ) ;
#14203 = CARTESIAN_POINT ( 'NONE',  ( -1.767766952966369765, 188.5000000000000000, 8.767766952966368876 ) ) ;
#14204 = CARTESIAN_POINT ( 'NONE',  ( 4.069800786343695798, -4.744882212776915686, 25.37381964045071925 ) ) ;
#14206 = ORIENTED_EDGE ( 'NONE', *, *, #4080, .T. ) ;
#14205 = CARTESIAN_POINT ( 'NONE',  ( 5.317509234264064411, -2.779225709350791274, 24.49999999999999289 ) ) ;
#14207 = CARTESIAN_POINT ( 'NONE',  ( -6.020865209844581400, 1.681180471732190984, 18.97400098023329562 ) ) ;
#14208 = CARTESIAN_POINT ( 'NONE',  ( 2.500000000000000444, 186.4500000000000171, 5.964466094067262247 ) ) ;
#14209 = CARTESIAN_POINT ( 'NONE',  ( -1.265664690411614835E-16, 2.066987299999999639, -2.949999998907525178 ) ) ;
#14210 =( NAMED_UNIT ( * ) PLANE_ANGLE_UNIT ( ) SI_UNIT ( $, .RADIAN. ) );
#14211 = CARTESIAN_POINT ( 'NONE',  ( 5.903472034603542085, 2.056448723545071022, 25.50008219321556524 ) ) ;
#14212 = CARTESIAN_POINT ( 'NONE',  ( -7.490007020835684592, -2.433650805992431110, 11.49999999999998224 ) ) ;
#14213 = CARTESIAN_POINT ( 'NONE',  ( 5.935543223013869607, -0.8771126767605967878, 11.49999999999998224 ) ) ;
#14214 = CARTESIAN_POINT ( 'NONE',  ( 0.5467140873060455375, 228.8869147685435053, 8.800851294624202126 ) ) ;
#14215 = CARTESIAN_POINT ( 'NONE',  ( -9.750000000000003553, 182.0000000000000000, -3.401296724241641415E-14 ) ) ;
#14216 = CYLINDRICAL_SURFACE ( 'NONE', #14654, 1.000000000000000888 ) ;
#14217 = CARTESIAN_POINT ( 'NONE',  ( -4.286401442266546624, -4.198423832313179282, 30.86935038651143870 ) ) ;
#14218 = VERTEX_POINT ( 'NONE', #14673 ) ;
#14219 = CARTESIAN_POINT ( 'NONE',  ( 1.461580736456472795, 184.9499999989075150, 8.461580736456474128 ) ) ;
#14220 = CARTESIAN_POINT ( 'NONE',  ( 2.692335458626878175, 5.362264153667219979, 30.73760108194402818 ) ) ;
#14221 = AXIS2_PLACEMENT_3D ( 'NONE', #14603, #13321, #7291 ) ;
#14222 = VERTEX_POINT ( 'NONE', #13545 ) ;
#14223 = CARTESIAN_POINT ( 'NONE',  ( -2.668367453516631738, -5.373994336898133106, 4.867606119983652668 ) ) ;
#14224 = CARTESIAN_POINT ( 'NONE',  ( -2.066987300000000083, 184.8499999989075206, 7.000000000000000000 ) ) ;
#14225 = CARTESIAN_POINT ( 'NONE',  ( 4.153440676704335921, 4.671190581744546044, 17.20045537531156654 ) ) ;
#14226 = CARTESIAN_POINT ( 'NONE',  ( 0.8561741729129457301, 186.7999999989075093, 4.933012699999999029 ) ) ;
#14227 = CARTESIAN_POINT ( 'NONE',  ( -0.9735954530123476225, 6.173909381474019575, 24.76281793585233615 ) ) ;
#14228 = CARTESIAN_POINT ( 'NONE',  ( 1.035533905932739085, -2.500000000000000000, 1.250000002184949999 ) ) ;
#14229 = CARTESIAN_POINT ( 'NONE',  ( -1.558540622947912624E-16, 189.0624999997268390, 4.500000000000000000 ) ) ;
#14230 = CARTESIAN_POINT ( 'NONE',  ( -5.999999999999999112, 227.2817795252328210, 4.165129161027028459 ) ) ;
#14231 = CARTESIAN_POINT ( 'NONE',  ( 1.035533905932737531, 2.500000000000000444, 0.6500000000000000222 ) ) ;
#14232 = CARTESIAN_POINT ( 'NONE',  ( -5.317509234263865459, -2.779225709351170526, 17.99999999999998934 ) ) ;
#14233 = CARTESIAN_POINT ( 'NONE',  ( 5.867109477881234270, 1.259218163100955135, 12.29888242247938202 ) ) ;
#14234 = ORIENTED_EDGE ( 'NONE', *, *, #10365, .F. ) ;
#14235 = ORIENTED_EDGE ( 'NONE', *, *, #10572, .T. ) ;
#14236 = ORIENTED_EDGE ( 'NONE', *, *, #2004, .F. ) ;
#14237 = CARTESIAN_POINT ( 'NONE',  ( 2.066987300000000083, 185.2499999989074979, 7.000000000000000000 ) ) ;
#14238 = CARTESIAN_POINT ( 'NONE',  ( 1.003991088089927430, 227.6914879785015273, 5.348390542306004747 ) ) ;
#14239 = ORIENTED_EDGE ( 'NONE', *, *, #1976, .F. ) ;
#14240 = CARTESIAN_POINT ( 'NONE',  ( 2.500000000000000000, 3.061616997868383141E-16, -1.799999997815050712 ) ) ;
#14241 = EDGE_CURVE ( 'NONE', #8559, #9290, #6170, .T. ) ;
#14242 = CARTESIAN_POINT ( 'NONE',  ( -0.9740807849834127730, 5.920620690450721924, 24.23850119700668770 ) ) ;
#14243 = DIRECTION ( 'NONE',  ( 0.000000000000000000, 0.000000000000000000, -1.000000000000000000 ) ) ;
#14244 = CARTESIAN_POINT ( 'NONE',  ( -2.066987300000000083, 184.7999999989075093, 6.143825827087054492 ) ) ;
#14245 = CARTESIAN_POINT ( 'NONE',  ( 1.035533905932739085, -2.500000000000000000, 0.3569999999781505173 ) ) ;
#14246 = EDGE_CURVE ( 'NONE', #7176, #7562, #15263, .T. ) ;
#14247 = CARTESIAN_POINT ( 'NONE',  ( 5.317509234263995133, 2.779225709350928497, 18.13236078583908650 ) ) ;
#14248 = ITEM_DEFINED_TRANSFORMATION ( 'NONE', 'NONE', #7627,  #14201 ) ;
#14249 = CARTESIAN_POINT ( 'NONE',  ( -2.066987299999999639, 0.8561741729129452860, -0.3999999989075250784 ) ) ;
#14250 = CARTESIAN_POINT ( 'NONE',  ( 4.286401442266483564, 4.198423832313243231, 11.49999999999998224 ) ) ;
#14251 = CARTESIAN_POINT ( 'NONE',  ( 2.961752869269595134, 227.1327854310254111, 6.866142280206398496 ) ) ;
#14252 = CARTESIAN_POINT ( 'NONE',  ( -1.767766952966369098, 1.767766952966369098, 0.9000000021849497989 ) ) ;
#14253 = ORIENTED_EDGE ( 'NONE', *, *, #7457, .T. ) ;
#14254 = CARTESIAN_POINT ( 'NONE',  ( -5.486741141153734347, 2.429871531109867533, 25.29888242247941221 ) ) ;
#14255 = VERTEX_POINT ( 'NONE', #12274 ) ;
#14256 = ORIENTED_EDGE ( 'NONE', *, *, #9015, .T. ) ;
#14257 = CARTESIAN_POINT ( 'NONE',  ( -5.570820891630772209, -2.833901239560386642, 30.73763026556126476 ) ) ;
#14258 = CARTESIAN_POINT ( 'NONE',  ( 2.066987300000000083, 184.4499999989075150, 7.000000000000000000 ) ) ;
#14259 = CARTESIAN_POINT ( 'NONE',  ( 1.000049271338486978, -6.169473353325553688, 4.869696127045518352 ) ) ;
#14260 = VERTEX_POINT ( 'NONE', #6483 ) ;
#14261 = CARTESIAN_POINT ( 'NONE',  ( -5.531623157106139388, 2.327208526676502132, 17.12635295315576300 ) ) ;
#14262 = CARTESIAN_POINT ( 'NONE',  ( 2.668367453516445220, 5.373994336898223700, 24.63064961348855064 ) ) ;
#14263 = CARTESIAN_POINT ( 'NONE',  ( 2.030576276931546336E-13, 6.000000000000000888, 25.49999999999999645 ) ) ;
#14264 = CARTESIAN_POINT ( 'NONE',  ( -2.997451966578492222, 5.485105005465963579, 12.11517780375842790 ) ) ;
#14265 = DIRECTION ( 'NONE',  ( 0.000000000000000000, 1.000000000000000000, 0.000000000000000000 ) ) ;
#14266 = CARTESIAN_POINT ( 'NONE',  ( -3.255013540813738615, -5.336859797930776139, 25.37381964045071214 ) ) ;
#14267 = DIRECTION ( 'NONE',  ( 1.000000000000000000, 0.000000000000000000, 0.000000000000000000 ) ) ;
#14268 = CARTESIAN_POINT ( 'NONE',  ( 2.500000000000000444, 184.7499999978150527, 5.964466094067262247 ) ) ;
#14269 = CARTESIAN_POINT ( 'NONE',  ( -0.5160604560792059203, 228.8899596144369752, 8.809644983231040172 ) ) ;
#14270 = CARTESIAN_POINT ( 'NONE',  ( -6.142908455506914223, -1.155755562476204590, 18.61517780375842790 ) ) ;
#14271 = CARTESIAN_POINT ( 'NONE',  ( 0.07962197837298144731, 190.0874091994478761, 4.202769589527701299 ) ) ;
#14272 = AXIS2_PLACEMENT_3D ( 'NONE', #11026, #12137, #124 ) ;
#14273 = CARTESIAN_POINT ( 'NONE',  ( 4.404571325722361763E-17, 185.7999999999999829, 4.500000000000000000 ) ) ;
#14274 = CARTESIAN_POINT ( 'NONE',  ( -3.736532060717997261, 4.696070028785964467, 4.026221760567070262 ) ) ;
#14276 = ORIENTED_EDGE ( 'NONE', *, *, #8137, .F. ) ;
#14275 = CARTESIAN_POINT ( 'NONE',  ( 6.123233995736766282E-16, -6.250000000000000888, 5.000000000000004441 ) ) ;
#14277 = FACE_OUTER_BOUND ( 'NONE', #6326, .T. ) ;
#14278 = EDGE_CURVE ( 'NONE', #25, #8865, #6541, .T. ) ;
#14279 = CARTESIAN_POINT ( 'NONE',  ( 5.131373506000491247, 7.062729720844170167, 17.99999999999998934 ) ) ;
#14280 = VERTEX_POINT ( 'NONE', #9175 ) ;
#14281 = CARTESIAN_POINT ( 'NONE',  ( 5.000000000000000000, 6.123233995736765296E-16, 36.00000000000000711 ) ) ;
#14282 = CARTESIAN_POINT ( 'NONE',  ( -2.999949572879441639, 227.1989808014691903, 7.061061364497972725 ) ) ;
#14283 = EDGE_CURVE ( 'NONE', #6446, #9498, #13852, .T. ) ;
#14284 = CONICAL_SURFACE ( 'NONE', #2615, 4.000000000000002665, 0.1745329251994333364 ) ;
#14285 = CYLINDRICAL_SURFACE ( 'NONE', #9808, 1.000000000000000666 ) ;
#14286 = CARTESIAN_POINT ( 'NONE',  ( -1.767766952966369765, 186.0300000002184788, 8.767766952966368876 ) ) ;
#14287 = CYLINDRICAL_SURFACE ( 'NONE', #930, 2.500000000000000000 ) ;
#14288 = B_SPLINE_CURVE_WITH_KNOTS ( 'NONE', 3,
 ( #3665, #2474, #86, #245, #5183, #8539, #9880, #8848, #1429, #8770, #7335, #9958, #12178, #13601, #6305, #2711, #6149, #10987 ),
 .UNSPECIFIED., .F., .F.,
 ( 4, 2, 2, 2, 2, 2, 2, 2, 4 ),
 ( 0.000000000000000000, 0.0003914898357794972241, 0.0007829796715589944483, 0.001174469507338491564, 0.001565959343117988897, 0.001957449178897486229, 0.002348939014676983128, 0.002740428850456480461, 0.003131918686235977793 ),
 .UNSPECIFIED. ) ;
#14289 = CARTESIAN_POINT ( 'NONE',  ( 1.237586355860756271, 228.7707919832083689, 8.465482067366952634 ) ) ;
#14290 = CARTESIAN_POINT ( 'NONE',  ( 5.770331821586398569, 2.404225004693612000, 10.62619944752603196 ) ) ;
#14291 = CARTESIAN_POINT ( 'NONE',  ( 0.8561741729129465073, -2.066987299999999195, -0.6999999989075250673 ) ) ;
#14292 = ADVANCED_FACE ( 'NONE', ( #1917, #5595 ), #726, .T. ) ;
#14293 = ORIENTED_EDGE ( 'NONE', *, *, #1458, .T. ) ;
#14294 = LINE ( 'NONE', #2287, #5301 ) ;
#14295 = CARTESIAN_POINT ( 'NONE',  ( 3.311576095066566694, 5.004818610361317255, 30.02622176056706493 ) ) ;
#14296 = ORIENTED_EDGE ( 'NONE', *, *, #12522, .F. ) ;
#14297 = CARTESIAN_POINT ( 'NONE',  ( -5.131373506000731055, 7.062729720844018289, 31.00000000000000000 ) ) ;
#14298 = FACE_OUTER_BOUND ( 'NONE', #1158, .T. ) ;
#14299 = CARTESIAN_POINT ( 'NONE',  ( 3.458623254138613046, 5.207221900902883505, 17.02622717124729945 ) ) ;
#14300 = CARTESIAN_POINT ( 'NONE',  ( 0.8561741729129461742, 185.6999999989075150, 9.066987300000000971 ) ) ;
#14301 = CARTESIAN_POINT ( 'NONE',  ( 3.922396193919000407, -4.541970110199484267, 18.87380682714709579 ) ) ;
#14302 = CARTESIAN_POINT ( 'NONE',  ( 2.500000000000000444, 1.035533905932737975, 0.6500000021849499099 ) ) ;
#14303 = CYLINDRICAL_SURFACE ( 'NONE', #13912, 1.500000000000000000 ) ;
#14304 = CARTESIAN_POINT ( 'NONE',  ( 5.999999999999999112, 222.7460571280668091, 12.08513476933103448 ) ) ;
#14305 = CARTESIAN_POINT ( 'NONE',  ( 7.799024015210652472, -1.482594289697024781, 11.49999999999998224 ) ) ;
#14306 = CARTESIAN_POINT ( 'NONE',  ( -2.500000000000000444, 185.0999999978150754, 7.000000000000000000 ) ) ;
#14307 = CIRCLE ( 'NONE', #343, 20.00000000000000000 ) ;
#14308 = CARTESIAN_POINT ( 'NONE',  ( 5.940390500375496430, 6.474944468551661281, 11.49999999999998224 ) ) ;
#14309 = ORIENTED_EDGE ( 'NONE', *, *, #7371, .T. ) ;
#14310 = B_SPLINE_CURVE_WITH_KNOTS ( 'NONE', 3,
 ( #3516, #5035, #13302, #2563, #4962, #6315, #13224, #6237, #1204, #8549, #10920, #2399, #2485, #11151, #8625, #12185, #1283, #6157 ),
 .UNSPECIFIED., .F., .F.,
 ( 4, 2, 2, 2, 2, 2, 2, 2, 4 ),
 ( 0.003131918686235973456, 0.003523310662250264159, 0.003914702638264554863, 0.004306094614278845566, 0.004697486590293136269, 0.005088878566307427839, 0.005480270542321719410, 0.005871662518336010980, 0.006263054494350302551 ),
 .UNSPECIFIED. ) ;
#14311 = ORIENTED_EDGE ( 'NONE', *, *, #2200, .T. ) ;
#14312 = EDGE_LOOP ( 'NONE', ( #14127, #14363, #9189, #8196 ) ) ;
#14313 = CARTESIAN_POINT ( 'NONE',  ( -2.066987300000000083, 184.7999999989075093, 6.143825827087054492 ) ) ;
#14314 = CARTESIAN_POINT ( 'NONE',  ( 6.176542424588105540, 0.9554180641286316167, 5.000000000000004441 ) ) ;
#14315 =( BOUNDED_SURFACE ( )  B_SPLINE_SURFACE ( 1, 2, ( 
 ( #9370, #10638, #11589, #3554, #13338, #2595, #9530, #7147, #1318, #3631, #13178, #11901, #2440, #8507, #5872, #8661, #9846, #1009, #14619, #9613, #7227, #4756, #1089, #13260, #11031, #9695, #2277, #4918, #129, #13417, #10719, #8340, #6194, #15577, #4995, #12220, #3708, #8585, #6032, #15654, #2523, #1163, #9774, #14696, #4837, #14451, #2359, #12145, #12065, #7303, #14365, #4677, #3784, #6116, #14532, #3471, #13492, #11983, #52, #8423, #10795, #1244, #10953, #5951, #10878, #10901, #7378, #15013, #366, #213, #519, #5390, #15088, #10237, #4105, #4183, #4020, #3862, #9054, #5314, #6269, #1475, #8896, #286, #13879, #11187, #11419, #7764, #3937, #7528, #6584, #7451, #12296, #12533, #1394, #6509, #8975, #7608, #11108, #5149, #14928 ),
 ( #10159, #11342, #13732, #5232, #2839, #5072, #8813, #9923, #14776, #10078, #1633, #2757, #13804, #2913, #7685, #12611, #8734, #13566, #2676, #10004, #6353, #439, #1707, #12374, #14851, #13641, #12456, #1556, #6433, #11265, #11804, #908, #10622, #5776, #10543, #15485, #15322, #15165, #4581, #833, #1788, #12760, #4422, #11573, #9432, #6740, #6971, #3299, #15241, #3068, #2101, #2992, #7846, #8082, #12691, #2022, #15401, #3146, #6663, #669, #10467, #11495, #4342, #598, #5469, #10312, #4262, #12841, #9199, #3219, #8161, #9130, #9277, #14115, #13961, #7919, #5699, #5543, #1866, #10393, #4497, #14039, #6896, #7999, #1943, #6818, #11653, #755, #5621, #12922, #11729, #9351, #14193, #12997, #11881, #9512, #3691, #6014, #15559, #4980, #4821 ) ),
 .UNSPECIFIED., .F., .F., .F. ) 
 B_SPLINE_SURFACE_WITH_KNOTS ( ( 2, 2 ),
 ( 3, 2, 2, 2, 2, 2, 2, 2, 2, 2, 2, 2, 2, 2, 2, 2, 2, 2, 2, 2, 2, 2, 2, 2, 2, 2, 2, 2, 2, 2, 2, 2, 2, 2, 2, 2, 2, 2, 2, 2, 2, 2, 2, 2, 2, 2, 2, 2, 2, 2, 3 ),
 ( 0.000000000000000000, 1.000000000000000000 ),
 ( 0.000000000000000000, 0.01785714285714285615, 0.03571428571428571230, 0.05357142857142856845, 0.07142857142857142461, 0.08928571428571428770, 0.1071428571428571369, 0.1250000000000000000, 0.1428571428571428492, 0.1607142857142857262, 0.1785714285714285754, 0.1964285714285714246, 0.2142857142857142738, 0.2321428571428571508, 0.2500000000000000000, 0.2678571428571428492, 0.2857142857142856984, 0.3035714285714285476, 0.3214285714285714524, 0.3392857142857143016, 0.3571428571428571508, 0.3750000000000000000, 0.3928571428571428492, 0.4107142857142856984, 0.4285714285714285476, 0.4464285714285714524, 0.4642857142857143016, 0.4821428571428571508, 0.5000000000000000000, 0.5178571428571429047, 0.5357142857142856984, 0.5535714285714286031, 0.5714285714285713969, 0.5892857142857143016, 0.6071428571428570953, 0.6250000000000000000, 0.6428571428571429047, 0.6607142857142856984, 0.6785714285714286031, 0.6964285714285713969, 0.7142857142857143016, 0.7321428571428570953, 0.7500000000000000000, 0.7678571428571429047, 0.7857142857142856984, 0.8035714285714286031, 0.8214285714285713969, 0.8392857142857143016, 0.8571428571428570953, 0.8750000000000000000, 0.8928571428571429047 ),
 .UNSPECIFIED. ) 
 GEOMETRIC_REPRESENTATION_ITEM ( )  RATIONAL_B_SPLINE_SURFACE ( (
 ( 1.000000000000000000, 0.9238795325112867385, 1.000000000000000000, 0.9238795325112867385, 1.000000000000000000, 0.9238795325112867385, 1.000000000000000000, 0.9238795325112867385, 1.000000000000000000, 0.9238795325112867385, 1.000000000000000000, 0.9238795325112867385, 1.000000000000000000, 0.9238795325112867385, 1.000000000000000000, 0.9238795325112867385, 1.000000000000000000, 0.9238795325112867385, 1.000000000000000000, 0.9238795325112867385, 1.000000000000000000, 0.9238795325112867385, 1.000000000000000000, 0.9238795325112867385, 1.000000000000000000, 0.9238795325112867385, 1.000000000000000000, 0.9238795325112867385, 1.000000000000000000, 0.9238795325112867385, 1.000000000000000000, 0.9238795325112867385, 1.000000000000000000, 0.9238795325112867385, 1.000000000000000000, 0.9238795325112867385, 1.000000000000000000, 0.9238795325112867385, 1.000000000000000000, 0.9238795325112867385, 1.000000000000000000, 0.9238795325112867385, 1.000000000000000000, 0.9238795325112867385, 1.000000000000000000, 0.9238795325112867385, 1.000000000000000000, 0.9238795325112867385, 1.000000000000000000, 0.9238795325112867385, 1.000000000000000000, 0.9238795325112867385, 1.000000000000000000, 0.9238795325112867385, 1.000000000000000000, 0.9238795325112867385, 1.000000000000000000, 0.9238795325112867385, 1.000000000000000000, 0.9238795325112867385, 1.000000000000000000, 0.9238795325112867385, 1.000000000000000000, 0.9238795325112867385, 1.000000000000000000, 0.9238795325112867385, 1.000000000000000000, 0.9238795325112867385, 1.000000000000000000, 0.9238795325112867385, 1.000000000000000000, 0.9238795325112867385, 1.000000000000000000, 0.9238795325112867385, 1.000000000000000000, 0.9238795325112867385, 1.000000000000000000, 0.9238795325112867385, 1.000000000000000000, 0.9238795325112867385, 1.000000000000000000, 0.9238795325112867385, 1.000000000000000000, 0.9238795325112867385, 1.000000000000000000, 0.9238795325112867385, 1.000000000000000000, 0.9238795325112867385, 1.000000000000000000, 0.9238795325112867385, 1.000000000000000000, 0.9238795325112867385, 1.000000000000000000, 0.9238795325112867385, 1.000000000000000000, 0.9238795325112867385, 1.000000000000000000, 0.9238795325112867385, 1.000000000000000000, 0.9238795325112867385, 1.000000000000000000),
 ( 1.000000000000000000, 0.9238795325112867385, 1.000000000000000000, 0.9238795325112867385, 1.000000000000000000, 0.9238795325112867385, 1.000000000000000000, 0.9238795325112867385, 1.000000000000000000, 0.9238795325112867385, 1.000000000000000000, 0.9238795325112867385, 1.000000000000000000, 0.9238795325112867385, 1.000000000000000000, 0.9238795325112867385, 1.000000000000000000, 0.9238795325112867385, 1.000000000000000000, 0.9238795325112867385, 1.000000000000000000, 0.9238795325112867385, 1.000000000000000000, 0.9238795325112867385, 1.000000000000000000, 0.9238795325112867385, 1.000000000000000000, 0.9238795325112867385, 1.000000000000000000, 0.9238795325112867385, 1.000000000000000000, 0.9238795325112867385, 1.000000000000000000, 0.9238795325112867385, 1.000000000000000000, 0.9238795325112867385, 1.000000000000000000, 0.9238795325112867385, 1.000000000000000000, 0.9238795325112867385, 1.000000000000000000, 0.9238795325112867385, 1.000000000000000000, 0.9238795325112867385, 1.000000000000000000, 0.9238795325112867385, 1.000000000000000000, 0.9238795325112867385, 1.000000000000000000, 0.9238795325112867385, 1.000000000000000000, 0.9238795325112867385, 1.000000000000000000, 0.9238795325112867385, 1.000000000000000000, 0.9238795325112867385, 1.000000000000000000, 0.9238795325112867385, 1.000000000000000000, 0.9238795325112867385, 1.000000000000000000, 0.9238795325112867385, 1.000000000000000000, 0.9238795325112867385, 1.000000000000000000, 0.9238795325112867385, 1.000000000000000000, 0.9238795325112867385, 1.000000000000000000, 0.9238795325112867385, 1.000000000000000000, 0.9238795325112867385, 1.000000000000000000, 0.9238795325112867385, 1.000000000000000000, 0.9238795325112867385, 1.000000000000000000, 0.9238795325112867385, 1.000000000000000000, 0.9238795325112867385, 1.000000000000000000, 0.9238795325112867385, 1.000000000000000000, 0.9238795325112867385, 1.000000000000000000, 0.9238795325112867385, 1.000000000000000000, 0.9238795325112867385, 1.000000000000000000, 0.9238795325112867385, 1.000000000000000000, 0.9238795325112867385, 1.000000000000000000, 0.9238795325112867385, 1.000000000000000000, 0.9238795325112867385, 1.000000000000000000, 0.9238795325112867385, 1.000000000000000000, 0.9238795325112867385, 1.000000000000000000) ) ) 
 REPRESENTATION_ITEM ( '' )  SURFACE ( )  );
#14316 = ORIENTED_EDGE ( 'NONE', *, *, #13811, .F. ) ;
#14317 = CARTESIAN_POINT ( 'NONE',  ( -1.035533905932738197, -2.500000000000000000, -1.249999997815050445 ) ) ;
#14318 = CARTESIAN_POINT ( 'NONE',  ( 6.123233995736766282E-16, -6.000000000000000888, 6.000000000000005329 ) ) ;
#14319 = CARTESIAN_POINT ( 'NONE',  ( 4.069684453406150482, 4.744965295353682500, 25.37380055247395561 ) ) ;
#14320 = CARTESIAN_POINT ( 'NONE',  ( -2.066987300000000083, 186.3999999989075320, 6.143825827087054492 ) ) ;
#14321 = CARTESIAN_POINT ( 'NONE',  ( -1.035533905932737753, 2.500000000000000444, 0.7569999999781505950 ) ) ;
#14322 = AXIS2_PLACEMENT_3D ( 'NONE', #7688, #8737, #6436 ) ;
#14323 = B_SPLINE_CURVE_WITH_KNOTS ( 'NONE', 3,
 ( #15434, #14223, #10424, #3250, #9545, #13195, #4534, #942, #3330, #705, #3488, #4695, #6772, #9465, #4452, #2055, #15356, #11689 ),
 .UNSPECIFIED., .F., .F.,
 ( 4, 2, 2, 2, 2, 2, 2, 2, 4 ),
 ( 0.000000000000000000, 0.0003914898357794969531, 0.0007829796715589939062, 0.001174469507338490913, 0.001565959343117987812, 0.001957449178897484494, 0.002348939014676980526, 0.002740428850456476557, 0.003131918686235972155 ),
 .UNSPECIFIED. ) ;
#14324 = CARTESIAN_POINT ( 'NONE',  ( 5.903472034603497676, -2.056448723545186485, 3.999917806784441865 ) ) ;
#14325 = EDGE_CURVE ( 'NONE', #3644, #3603, #6713, .T. ) ;
#14326 = CARTESIAN_POINT ( 'NONE',  ( -0.8561741729129458411, -2.066987299999999195, -0.1999999989075254836 ) ) ;
#14327 = CARTESIAN_POINT ( 'NONE',  ( -2.500000000000000444, 1.035533905932737753, -2.350000000000000533 ) ) ;
#14328 = CARTESIAN_POINT ( 'NONE',  ( 2.053141855112443626, 226.5855735425530497, 5.254201149538955562 ) ) ;
#14329 = CARTESIAN_POINT ( 'NONE',  ( 6.172614129015222773, 0.9817721000789578767, 5.262369734438754776 ) ) ;
#14330 = ORIENTED_EDGE ( 'NONE', *, *, #748, .F. ) ;
#14331 = VERTEX_POINT ( 'NONE', #11395 ) ;
#14332 = DIRECTION ( 'NONE',  ( 1.000000000000000000, 0.000000000000000000, 0.000000000000000000 ) ) ;
#14333 = ORIENTED_EDGE ( 'NONE', *, *, #2290, .F. ) ;
#14334 =( BOUNDED_CURVE ( )  B_SPLINE_CURVE ( 2, ( #6708, #410, #5433, #7809, #15209, #1524, #11537, #14980, #12580 ),
 .UNSPECIFIED., .F., .F. ) 
 B_SPLINE_CURVE_WITH_KNOTS ( ( 3, 2, 2, 2, 3 ),
 ( 0.2857142857142856984, 0.3035714285714285476, 0.3214285714285715079, 0.3392857142857143571, 0.3571428571428572063 ),
 .UNSPECIFIED. ) 
 CURVE ( )  GEOMETRIC_REPRESENTATION_ITEM ( )  RATIONAL_B_SPLINE_CURVE ( ( 1.000000000000000000, 0.9238795325112867385, 1.000000000000000000, 0.9238795325112867385, 1.000000000000000000, 0.9238795325112867385, 1.000000000000000000, 0.9238795325112865164, 1.000000000000000222 ) ) 
 REPRESENTATION_ITEM ( '' )  );
#14335 = VERTEX_POINT ( 'NONE', #9251 ) ;
#14336 = ADVANCED_FACE ( 'NONE', ( #6557, #15215 ), #805, .T. ) ;
#14337 = CARTESIAN_POINT ( 'NONE',  ( 1.354942164753511828E-13, -6.250000000000000888, 16.99999999999998579 ) ) ;
#14338 = AXIS2_PLACEMENT_3D ( 'NONE', #9496, #9661, #9745 ) ;
#14339 = CARTESIAN_POINT ( 'NONE',  ( -2.817313151351291012, -5.579000502529382288, 24.36762589283694780 ) ) ;
#14340 = CARTESIAN_POINT ( 'NONE',  ( -4.142620314836442219, -4.341347824677446177, 25.11442521571937547 ) ) ;
#14341 = EDGE_LOOP ( 'NONE', ( #7893, #9067, #13701, #6164, #9103, #609 ) ) ;
#14342 = CARTESIAN_POINT ( 'NONE',  ( -6.142844459177249306, 1.156093792145143961, 31.61560192892921251 ) ) ;
#14343 = CARTESIAN_POINT ( 'NONE',  ( 3.736691294293271959, 4.695920479336495923, 25.47358595436692852 ) ) ;
#14344 = CARTESIAN_POINT ( 'NONE',  ( -2.668367453516691690, -5.373994336898102020, 11.49999999999998224 ) ) ;
#14345 = CARTESIAN_POINT ( 'NONE',  ( -4.435347140101121965, 4.403429997944423135, 11.63063932754213070 ) ) ;
#14346 = CARTESIAN_POINT ( 'NONE',  ( -6.172552660730949547, -0.9821660343540521421, 24.23620383159192926 ) ) ;
#14347 = DIRECTION ( 'NONE',  ( -0.000000000000000000, -1.000000000000000000, -0.000000000000000000 ) ) ;
#14348 = CARTESIAN_POINT ( 'NONE',  ( -1.035533905932739751, 189.2499999978150811, 9.500000000000003553 ) ) ;
#14349 = CLOSED_SHELL ( 'NONE', ( #10212, #1823, #15565, #3854, #5372, #6826, #6651, #7081, #4849, #1622, #3267, #9338, #12644, #3814, #1519, #9461, #6599 ) ) ;
#14350 = CARTESIAN_POINT ( 'NONE',  ( 0.4870669733929915424, 228.2428440931186628, 10.13214456346285708 ) ) ;
#14351 = CARTESIAN_POINT ( 'NONE',  ( -6.172639027853096927, -0.9816353142772993312, 18.26225281721714566 ) ) ;
#14352 = EDGE_CURVE ( 'NONE', #12581, #4214, #14956, .T. ) ;
#14353 = DIRECTION ( 'NONE',  ( 1.000000000000000000, -3.326610055774643275E-18, 1.062480551894329622E-17 ) ) ;
#14354 = ORIENTED_EDGE ( 'NONE', *, *, #8973, .T. ) ;
#14355 = CARTESIAN_POINT ( 'NONE',  ( -5.746996058422770837, 1.729015645941936796, 12.50007961174474858 ) ) ;
#14356 = CARTESIAN_POINT ( 'NONE',  ( -0.7995298244853823455, -5.947211616899259923, 12.11456014619857946 ) ) ;
#14358 = ORIENTED_EDGE ( 'NONE', *, *, #2498, .F. ) ;
#14357 = DIRECTION ( 'NONE',  ( -1.000000000000000000, 0.000000000000000000, 0.000000000000000000 ) ) ;
#14359 = CARTESIAN_POINT ( 'NONE',  ( 0.08043465938667249127, -0.3999999999999898637, 2.550888629652776185 ) ) ;
#14360 = CARTESIAN_POINT ( 'NONE',  ( -6.176542424588100211, 0.9554180641286806885, 17.99999999999998934 ) ) ;
#14361 = CIRCLE ( 'NONE', #2688, 1.999999999999999556 ) ;
#14362 = EDGE_CURVE ( 'NONE', #5008, #12192, #2966, .T. ) ;
#14363 = ORIENTED_EDGE ( 'NONE', *, *, #1853, .T. ) ;
#14364 = CARTESIAN_POINT ( 'NONE',  ( -5.935543223013843850, -0.8771126767607685393, 31.00000000000000000 ) ) ;
#14365 = CARTESIAN_POINT ( 'NONE',  ( -1.461580736456472795, 1.461580736456472795, -0.2499999989075251672 ) ) ;
#14366 = CARTESIAN_POINT ( 'NONE',  ( -2.137511978810349156, 226.6127469305739339, 5.334277523823343081 ) ) ;
#14367 = CARTESIAN_POINT ( 'NONE',  ( 0.000000000000000000, 0.000000000000000000, 0.000000000000000000 ) ) ;
#14368 = CARTESIAN_POINT ( 'NONE',  ( -2.500000000000000000, 0.000000000000000000, -0.5999999978150503122 ) ) ;
#14369 = EDGE_CURVE ( 'NONE', #12563, #8014, #977, .T. ) ;
#14370 = CARTESIAN_POINT ( 'NONE',  ( 1.767766952966368432, 186.2300000002184959, 8.767766952966368876 ) ) ;
#14371 = CARTESIAN_POINT ( 'NONE',  ( -1.001898788273069663, 228.8297312643339296, 8.635702072933472806 ) ) ;
#14372 = CARTESIAN_POINT ( 'NONE',  ( -1.864073305829632599, 228.0308260764439297, 6.328418323741104246 ) ) ;
#14373 = DIRECTION ( 'NONE',  ( -1.000000000000000000, 0.000000000000000000, 0.000000000000000000 ) ) ;
#14374 = CARTESIAN_POINT ( 'NONE',  ( 1.461580736456472573, 1.461580736456472795, 1.150000001092474911 ) ) ;
#14375 = CARTESIAN_POINT ( 'NONE',  ( 6.176542424588126856, 0.9554180641284961695, 17.86936067245787285 ) ) ;
#14376 = ORIENTED_EDGE ( 'NONE', *, *, #11933, .F. ) ;
#14378 = B_SPLINE_SURFACE_WITH_KNOTS ( 'NONE', 1, 3, ( 
 ( #8429, #2601, #3791, #6200, #13425, #12226, #3561, #1249, #7534, #1480, #9853, #12381, #219, #9701, #4846, #12072, #6125, #7459, #1325, #6358, #7318, #2446, #9930, #10960, #9621, #5000, #6275, #14702, #1400, #13343, #3637, #14460, #13266, #11115, #5077, #14781, #2365, #3867, #7233, #8666, #9779, #8512, #1170, #7310, #12150, #13497, #57, #11037, #6039, #8741, #4924, #10884, #14625, #3714, #8591, #2529, #7384, #11499, #13967, #11425, #15018, #12696, #4268, #5318, #2845, #6439, #7691, #6746, #3073, #4110, #6589, #1638, #5155, #10241, #12461, #1871, #5239, #12541, #13737, #13648, #6515, #15093, #10316, #14936, #2997, #293, #14857, #8902, #12616, #15169, #9133, #8980, #1714, #11348, #7923, #2763, #13809, #10085, #12766, #10010, #4026, #3944, #525, #7852, #447, #1562, #7770, #5394, #7616, #11271, #8818, #4188, #9059, #371, #10163, #2920, #13884, #1792, #6668, #602, #5474, #5704, #15327, #761, #11579, #1950, #8090, #4502, #14119, #12927, #11809, #2027, #6977, #14043, #4347, #9517, #5781, #14197, #674, #912, #9283, #3379, #5626, #6824, #11658, #3225, #15405, #10397, #10473, #2181, #8247, #6903, #11736, #3459, #4426, #9358, #839, #14269, #7052, #8167, #8005, #8325, #9437, #3304 ),
 ( #10548, #13004, #2263, #9205, #14350, #10629, #13164, #15491, #5550, #4587, #13082, #2106, #11887, #996, #5859, #10706, #15563, #4665, #15247, #3152, #12847, #1231, #13323, #7366, #7441, #5937, #9835, #12208, #40, #13556, #3850, #15728, #12131, #196, #9913, #6019, #7134, #6100, #4984, #3696, #10784, #11098, #15643, #8651, #10942, #13481, #8573, #11970, #4744, #2345, #2513, #2585, #8723, #2424, #12285, #1151, #6181, #13402, #5060, #1076, #14684, #4825, #9595, #1305, #11019, #119, #3619, #8496, #3774, #14605, #14438, #7214, #9681, #1385, #7293, #14766, #6260, #3541, #8412, #13247, #14520, #10860, #12052, #4906, #9763, #508, #13866, #11175, #10224, #10301, #2902, #7675, #1545, #5138, #5219, #12445, #1696, #6420, #15002, #7518, #12679, #4008, #1777, #10069, #354, #1621, #4092, #8962, #2978, #585, #13793, #6497, #15075, #6650, #12523, #14918, #8803, #8887, #9116, #5454, #11332, #7751, #13719, #12364, #12597, #14840, #4248, #7597, #2826, #429, #276, #5300, #6572, #11483, #11253, #5378, #2665, #1461, #10148, #11407, #15153, #6339, #4169, #9041, #7829, #9991, #3926, #13632, #2746, #5840, #4644, #3134, #7907, #9337, #893, #7988, #15227, #5685, #10532, #12983, #15387, #4411, #5764, #4331 ) ),
 .UNSPECIFIED., .F., .T., .F.,
 ( 2, 2 ),
 ( 4, 2, 2, 2, 2, 2, 2, 2, 2, 2, 2, 2, 2, 2, 2, 2, 2, 2, 2, 2, 2, 2, 2, 2, 2, 2, 2, 2, 2, 2, 2, 2, 2, 2, 2, 2, 2, 2, 2, 2, 2, 2, 2, 2, 2, 2, 2, 2, 2, 2, 2, 2, 2, 2, 2, 2, 2, 2, 2, 2, 2, 2, 2, 2, 2, 2, 2, 2, 2, 2, 2, 2, 2, 2, 2, 2, 2, 2, 2, 2, 2, 4 ),
 ( 0.000000000000000000, 1.000000000000000000 ),
 ( 0.0002080168337970193793, 0.0004025046291346534252, 0.0005969924244722874711, 0.0006942363221411045754, 0.0007914802198099215712, 0.0009859680151475555630, 0.001180455810485189772, 0.001277699708154006767, 0.001374943605822823763, 0.001472187503491640759, 0.001569431401160457755, 0.001763919196498091747, 0.001958406991835725738, 0.002055650889504542951, 0.002152894787173360164, 0.002347382582510994155, 0.002541870377848628147, 0.002639114275517445360, 0.002736358173186262139, 0.002930845968523896131, 0.003125333763861530122, 0.003222577661530346901, 0.003319821559199164114, 0.003417065456867981327, 0.003514309354536798539, 0.003708797149874432531, 0.003903284945212066523, 0.004097772740549700948, 0.004292260535887335374, 0.004486748331224968932, 0.004681236126562602490, 0.004875723921900236915, 0.005070211717237871341, 0.005264699512575504899, 0.005361943410244322111, 0.005459187307913138457, 0.005653675103250772882, 0.005848162898588407307, 0.005945406796257223653, 0.006042650693926040865, 0.006237138489263674423, 0.006431626284601308849, 0.006626114079938943274, 0.006820601875276577700, 0.007015089670614212125, 0.007112333568283028470, 0.007209577465951845683, 0.007404065261289479241, 0.007598553056627113667, 0.007695796954295930879, 0.007793040851964748092, 0.007890284749633564437, 0.007987528647302382517, 0.008182016442640016943, 0.008376504237977651368, 0.008473748135646467713, 0.008570992033315284059, 0.008765479828652918484, 0.008959967623990552910, 0.009057211521659369255, 0.009154455419328185600, 0.009348943214665820026, 0.009543431010003454451, 0.009640674907672272531, 0.009737918805341088876, 0.009835162703009905222, 0.009932406600678723302, 0.01012689439601635599, 0.01032138219135399042, 0.01041862608902280676, 0.01051586998669162484, 0.01071035778202925753, 0.01090484557736689196, 0.01109933337270452638, 0.01129382116804216081, 0.01148830896337979524, 0.01168279675871742793, 0.01187728455405506235, 0.01207177234939269678, 0.01226626014473032947, 0.01246074794006796389, 0.01265523573540559832 ),
 .UNSPECIFIED. ) ;
#14377 = CARTESIAN_POINT ( 'NONE',  ( -2.066987300000000971, 188.6499999989075036, 7.000000000000000000 ) ) ;
#14379 = CARTESIAN_POINT ( 'NONE',  ( 1.461580736456472795, 184.9499999989075150, 8.461580736456474128 ) ) ;
#14380 = CARTESIAN_POINT ( 'NONE',  ( 5.866817325727539334, 1.260653813891824182, 23.69977782616121331 ) ) ;
#14381 = EDGE_LOOP ( 'NONE', ( #10908, #3347 ) ) ;
#14382 = EDGE_CURVE ( 'NONE', #13449, #8559, #5556, .T. ) ;
#14383 = CARTESIAN_POINT ( 'NONE',  ( -9.750000000000003553, 22.00000000000000000, -3.401296724241641415E-14 ) ) ;
#14384 = CARTESIAN_POINT ( 'NONE',  ( 5.486982057989181705, -2.429327048029897629, 5.799318062581740207 ) ) ;
#14385 = CARTESIAN_POINT ( 'NONE',  ( -4.267992336621205141, 4.217442018459991893, 31.26194324003147429 ) ) ;
#14386 = AXIS2_PLACEMENT_3D ( 'NONE', #4048, #9875, #8919 ) ;
#14387 = CARTESIAN_POINT ( 'NONE',  ( 5.999999999999999112, 222.7460571280668091, 12.08513476933103448 ) ) ;
#14388 = EDGE_CURVE ( 'NONE', #5635, #8014, #9102, .T. ) ;
#14389 = CARTESIAN_POINT ( 'NONE',  ( -1.461580736456473906, 186.3499999989074922, 8.461580736456474128 ) ) ;
#14390 = CARTESIAN_POINT ( 'NONE',  ( 3.632753594129205510, 4.777047695051075848, 18.99995053646221521 ) ) ;
#14391 = CARTESIAN_POINT ( 'NONE',  ( -2.500000000000000000, -1.035533905932739307, 0.2500000021849496656 ) ) ;
#14392 = CARTESIAN_POINT ( 'NONE',  ( 4.267936573529251376, -4.217499624512195844, 11.23770962164068798 ) ) ;
#14393 = CARTESIAN_POINT ( 'NONE',  ( 1.423015351387224570E-16, 184.1999999999999886, 4.500000000000000000 ) ) ;
#14394 = CARTESIAN_POINT ( 'NONE',  ( 0.2622538972264353285, -6.245673238944475791, 31.97385994369199835 ) ) ;
#14395 = CARTESIAN_POINT ( 'NONE',  ( -6.172639027853123572, 0.9816353142771289120, 11.23774718278287743 ) ) ;
#14396 = CARTESIAN_POINT ( 'NONE',  ( -1.000079958708000483, -5.916066267613719454, 18.13152738882033432 ) ) ;
#14397 = ORIENTED_EDGE ( 'NONE', *, *, #1458, .F. ) ;
#14398 = ORIENTED_EDGE ( 'NONE', *, *, #1654, .T. ) ;
#14399 = ORIENTED_EDGE ( 'NONE', *, *, #1804, .F. ) ;
#14400 = CARTESIAN_POINT ( 'NONE',  ( -3.311384659207207370, 5.004923837169374501, 12.47358595436692852 ) ) ;
#14401 = VERTEX_POINT ( 'NONE', #6791 ) ;
#14402 = ADVANCED_FACE ( 'NONE', ( #5671 ), #11625, .F. ) ;
#14403 = PRODUCT_DEFINITION_SHAPE ( 'NONE', 'NONE',  #15732 ) ;
#14404 = CARTESIAN_POINT ( 'NONE',  ( -1.035533905932737753, 2.500000000000000444, -3.149999997815050801 ) ) ;
#14405 = B_SPLINE_CURVE_WITH_KNOTS ( 'NONE', 3,
 ( #4028, #8904, #8743, #2847, #449, #5396, #5158, #8984, #221, #5080, #14859, #13888, #4192, #7855, #7695, #1641, #6517, #11117 ),
 .UNSPECIFIED., .F., .F.,
 ( 4, 2, 2, 2, 2, 2, 2, 2, 4 ),
 ( 0.000000000000000000, 0.0003914357524127460761, 0.0007828715048254921522, 0.001174307257238238174, 0.001565743009650984304, 0.001957178762063730218, 0.002348614514476476348, 0.002740050266889222479, 0.003131486019301968609 ),
 .UNSPECIFIED. ) ;
#14406 = DIRECTION ( 'NONE',  ( 0.000000000000000000, 1.000000000000000000, 0.000000000000000000 ) ) ;
#14407 = AXIS2_PLACEMENT_3D ( 'NONE', #1072, #8649, #2581 ) ;
#14408 = CARTESIAN_POINT ( 'NONE',  ( 5.726049995854435970, 2.506679546901950051, 31.79954462468841214 ) ) ;
#14409 = CARTESIAN_POINT ( 'NONE',  ( 2.066987299999999639, 188.4999999989074979, 6.143825827087054492 ) ) ;
#14410 = CARTESIAN_POINT ( 'NONE',  ( -2.500000000000000000, 0.000000000000000000, 0.9069999999781503952 ) ) ;
#14411 = VECTOR ( 'NONE', #7126, 1000.000000000000000 ) ;
#14412 = CARTESIAN_POINT ( 'NONE',  ( 5.571002711501416016, -2.833546409886269934, 4.736203831591940805 ) ) ;
#14413 = CARTESIAN_POINT ( 'NONE',  ( -2.066987299999999195, -0.8561741729129466183, -1.899999998907525800 ) ) ;
#14414 = CARTESIAN_POINT ( 'NONE',  ( 2.999999999999999556, -1.732050807568877859, -5.500000000000000000 ) ) ;
#14415 = CARTESIAN_POINT ( 'NONE',  ( -0.4900172623563870955, 226.3376062179358996, 4.523300904952406221 ) ) ;
#14416 = LINE ( 'NONE', #13381, #9270 ) ;
#14417 = ORIENTED_EDGE ( 'NONE', *, *, #1139, .T. ) ;
#14418 = ORIENTED_EDGE ( 'NONE', *, *, #553, .F. ) ;
#14419 = CYLINDRICAL_SURFACE ( 'NONE', #11379, 1.000000000000000888 ) ;
#14420 = CIRCLE ( 'NONE', #9117, 2.583009025355586186 ) ;
#14421 = ORIENTED_EDGE ( 'NONE', *, *, #13611, .T. ) ;
#14422 = EDGE_LOOP ( 'NONE', ( #3820, #12735 ) ) ;
#14423 = CARTESIAN_POINT ( 'NONE',  ( -6.142844459177229766, -1.156093792145233001, 30.38439807107076973 ) ) ;
#14424 = CIRCLE ( 'NONE', #5303, 20.00000000000000000 ) ;
#14425 = EDGE_CURVE ( 'NONE', #13467, #10770, #11452, .T. ) ;
#14426 = PLANE ( 'NONE',  #8392 ) ;
#14427 = CARTESIAN_POINT ( 'NONE',  ( -3.011385983131470212, -5.190390249166353165, 25.29952054102714953 ) ) ;
#14428 = CARTESIAN_POINT ( 'NONE',  ( 4.267558728637206755, -4.217879122113790125, 11.76382603205595423 ) ) ;
#14429 = UNCERTAINTY_MEASURE_WITH_UNIT (LENGTH_MEASURE( 1.000000000000000082E-05 ), #6034, 'distance_accuracy_value', 'NONE');
#14430 = CARTESIAN_POINT ( 'NONE',  ( 2.848235266350816808, 5.281699484015757839, 25.11397738943081848 ) ) ;
#14431 = DIRECTION ( 'NONE',  ( 1.000000000000000000, 0.000000000000000000, 0.000000000000000000 ) ) ;
#14432 = CARTESIAN_POINT ( 'NONE',  ( -3.882673863916337176, 4.899192824800900681, 12.47408542334169113 ) ) ;
#14433 = CARTESIAN_POINT ( 'NONE',  ( -5.648794263291666340, -2.676232015153777510, 23.88558052754514094 ) ) ;
#14434 = FACE_OUTER_BOUND ( 'NONE', #412, .T. ) ;
#14435 = CARTESIAN_POINT ( 'NONE',  ( 0.000000000000000000, 24.00000000000000000, 0.000000000000000000 ) ) ;
#14436 = AXIS2_PLACEMENT_3D ( 'NONE', #12891, #5439, #644 ) ;
#14437 = CARTESIAN_POINT ( 'NONE',  ( 1.035533905932737753, 187.2499999978151095, 4.500000000000000888 ) ) ;
#14438 = CARTESIAN_POINT ( 'NONE',  ( 1.458867243353906273, 226.4466662005724800, 4.844797864602860216 ) ) ;
#14439 = CARTESIAN_POINT ( 'NONE',  ( 2.668367453516610865, 5.373994336898140212, 31.00000000000000000 ) ) ;
#14440 = CARTESIAN_POINT ( 'NONE',  ( 5.935543223013849179, 0.8771126767607271280, 31.00000000000000000 ) ) ;
#14441 = EDGE_LOOP ( 'NONE', ( #15413, #5103, #4137, #13144 ) ) ;
#14442 = DIRECTION ( 'NONE',  ( -0.000000000000000000, -1.000000000000000000, -0.000000000000000000 ) ) ;
#14443 = CARTESIAN_POINT ( 'NONE',  ( 0.8002302970947245964, -5.947135855825854023, 10.88601773212297985 ) ) ;
#14444 =( GEOMETRIC_REPRESENTATION_CONTEXT ( 3 ) GLOBAL_UNCERTAINTY_ASSIGNED_CONTEXT ( ( #3448 ) ) GLOBAL_UNIT_ASSIGNED_CONTEXT ( ( #15296, #807, #10364 ) ) REPRESENTATION_CONTEXT ( 'NONE', 'WORKASPACE' ) );
#14446 = EDGE_LOOP ( 'NONE', ( #9229, #4710, #15625, #3342 ) ) ;
#14445 = CARTESIAN_POINT ( 'NONE',  ( -1.500000000000000000, 9.750000000000003553, 0.000000000000000000 ) ) ;
#14447 = CARTESIAN_POINT ( 'NONE',  ( 0.03145189498340861256, -0.3999999999999923617, 2.524708160309380389 ) ) ;
#14448 = COLOUR_RGB ( '', 0.66274510, 0.83137255, 0.94901961) ;
#14449 = CYLINDRICAL_SURFACE ( 'NONE', #9707, 1.000000000000000666 ) ;
#14450 = LINE ( 'NONE', #4994, #4368 ) ;
#14451 = CARTESIAN_POINT ( 'NONE',  ( -0.8561741729129458411, -2.066987299999999195, 1.092474635061568626E-09 ) ) ;
#14452 = CARTESIAN_POINT ( 'NONE',  ( -2.776549226834668538, 226.9241846788892190, 6.251816468300146035 ) ) ;
#14453 = EDGE_CURVE ( 'NONE', #2012, #5925, #11091, .T. ) ;
#14454 = DIRECTION ( 'NONE',  ( 0.9510565162951499785, 0.3090169943749582204, 0.000000000000000000 ) ) ;
#14455 = CARTESIAN_POINT ( 'NONE',  ( 1.035533905932738197, 188.5800000002184902, 9.500000000000003553 ) ) ;
#14456 = CARTESIAN_POINT ( 'NONE',  ( -4.291255145204061705, 4.544933371694689583, 5.613961794080712053 ) ) ;
#14457 = EDGE_CURVE ( 'NONE', #2406, #12251, #10, .T. ) ;
#14458 = CARTESIAN_POINT ( 'NONE',  ( -0.4523656679209748233, 227.6256624317788635, 5.158282608927489576 ) ) ;
#14460 = CARTESIAN_POINT ( 'NONE',  ( 1.785787022451674089, 228.5490719641819908, 7.825142006337427070 ) ) ;
#14459 = STYLED_ITEM ( 'NONE', ( #926 ), #8222 ) ;
#14461 = CARTESIAN_POINT ( 'NONE',  ( 3.796994071234844259E-16, -2.066987299999999639, 0.8500000010924748661 ) ) ;
#14462 = CIRCLE ( 'NONE', #6605, 2.499999999999999556 ) ;
#14463 = DIRECTION ( 'NONE',  ( 0.5000000000000000000, -0.8660254037844387076, 0.000000000000000000 ) ) ;
#14464 = EDGE_CURVE ( 'NONE', #3723, #1738, #9941, .T. ) ;
#14465 = ORIENTED_EDGE ( 'NONE', *, *, #5042, .F. ) ;
#14466 = CARTESIAN_POINT ( 'NONE',  ( 0.000000000000000000, 22.00000000000000000, -5.000000000000000000 ) ) ;
#14467 = CARTESIAN_POINT ( 'NONE',  ( 0.8561741729129461742, 186.4999999989075263, 9.066987300000000971 ) ) ;
#14468 = FACE_OUTER_BOUND ( 'NONE', #1504, .T. ) ;
#14469 = ORIENTED_EDGE ( 'NONE', *, *, #14382, .T. ) ;
#14470 = B_SPLINE_CURVE_WITH_KNOTS ( 'NONE', 3,
 ( #10288, #5597, #1765, #13934, #10521, #6871, #11547, #14015, #3045, #10211, #1920, #12668, #5673, #574, #9105, #4236, #13855, #7898 ),
 .UNSPECIFIED., .F., .F.,
 ( 4, 2, 2, 2, 2, 2, 2, 2, 4 ),
 ( 0.000000000000000000, 0.0003914898357794965736, 0.0007829796715589931472, 0.001174469507338489829, 0.001565959343117986294, 0.001957449178897482760, 0.002348939014676979659, 0.002740428850456476124, 0.003131918686235972589 ),
 .UNSPECIFIED. ) ;
#14471 = EDGE_CURVE ( 'NONE', #2830, #12811, #15634, .T. ) ;
#14472 = COLOUR_RGB ( '', 0.09019608, 0.27058824, 0.51372549) ;
#14473 = CARTESIAN_POINT ( 'NONE',  ( 0.5039005892423336075, -6.230833003620525723, 23.62636388911297303 ) ) ;
#14474 = COLOUR_RGB ( '', 0.09019608, 0.27058824, 0.51372549) ;
#14475 = CARTESIAN_POINT ( 'NONE',  ( 0.9999171162590435591, 6.169494774098537526, 11.36722320330675906 ) ) ;
#14476 = CARTESIAN_POINT ( 'NONE',  ( 5.082197683525802034E-17, 185.2499999989074979, 4.933012699999999029 ) ) ;
#14477 = CARTESIAN_POINT ( 'NONE',  ( 3.419318284370187477, -4.932111238568182898, 18.99992002356260201 ) ) ;
#14478 = CARTESIAN_POINT ( 'NONE',  ( 0.2265647620681634500, 189.0000000000732996, 9.493607781726925765 ) ) ;
#14479 = CARTESIAN_POINT ( 'NONE',  ( -0.7988914244718040569, -5.947301735519289423, 30.38456289168619051 ) ) ;
#14480 = CARTESIAN_POINT ( 'NONE',  ( -1.767766952966369098, 184.2999999999999829, 5.232233047033630235 ) ) ;
#14481 = CARTESIAN_POINT ( 'NONE',  ( 0.7993401192312087344, -6.199366368793657323, 31.61483246936573721 ) ) ;
#14482 = CARTESIAN_POINT ( 'NONE',  ( -6.176542424588111757, 0.9554180641286128539, 11.36762589283694425 ) ) ;
#14483 = CARTESIAN_POINT ( 'NONE',  ( -5.783239563508432823, 1.602707436861086299, 30.02641404563305016 ) ) ;
#14484 = ORIENTED_EDGE ( 'NONE', *, *, #8988, .F. ) ;
#14485 = MECHANICAL_DESIGN_GEOMETRIC_PRESENTATION_REPRESENTATION (  '', ( #13213 ), #4573 ) ;
#14486 = ORIENTED_EDGE ( 'NONE', *, *, #639, .F. ) ;
#14487 = ORIENTED_EDGE ( 'NONE', *, *, #12425, .T. ) ;
#14488 = CARTESIAN_POINT ( 'NONE',  ( -3.107688324358770071, 5.133887830459799240, 12.37378430870260715 ) ) ;
#14489 = VERTEX_POINT ( 'NONE', #12020 ) ;
#14490 = ADVANCED_FACE ( 'NONE', ( #8214 ), #2391, .F. ) ;
#14491 = CARTESIAN_POINT ( 'NONE',  ( -0.8561741729129458411, -2.066987299999999195, 1.400000001092474911 ) ) ;
#14492 = DIRECTION ( 'NONE',  ( 0.000000000000000000, 0.000000000000000000, 1.000000000000000000 ) ) ;
#14493 = CARTESIAN_POINT ( 'NONE',  ( 6.021135683317684339, 1.680226122398269295, 31.97377282875269700 ) ) ;
#14494 = CARTESIAN_POINT ( 'NONE',  ( -2.066987300000000971, 188.7999999989075093, 6.143825827087054492 ) ) ;
#14495 = CARTESIAN_POINT ( 'NONE',  ( 1.767766952966368654, 1.767766952966369098, -1.793000000021849338 ) ) ;
#14496 = CARTESIAN_POINT ( 'NONE',  ( -2.668367453516692134, -5.373994336898103796, 11.36760611998364467 ) ) ;
#14497 = ITEM_DEFINED_TRANSFORMATION ( 'NONE', 'NONE', #14407,  #14201 ) ;
#14498 = CARTESIAN_POINT ( 'NONE',  ( 1.461580736456473018, -1.461580736456472573, -1.649999998907525356 ) ) ;
#14499 = ADVANCED_FACE ( 'NONE', ( #5985 ), #1195, .F. ) ;
#14500 = CARTESIAN_POINT ( 'NONE',  ( 2.817313151351187983, -5.579000502529432914, 4.869360672457872852 ) ) ;
#14501 = CARTESIAN_POINT ( 'NONE',  ( -1.707413668510289861, 226.4963546398602148, 4.991255295473766118 ) ) ;
#14502 = CARTESIAN_POINT ( 'NONE',  ( -2.500000000000000000, 0.000000000000000000, 2.500000000000000000 ) ) ;
#14503 = ORIENTED_EDGE ( 'NONE', *, *, #5497, .T. ) ;
#14504 = ORIENTED_EDGE ( 'NONE', *, *, #993, .F. ) ;
#14505 = CARTESIAN_POINT ( 'NONE',  ( -1.084202172485504434E-15, -3.464101615137755275, -5.500000000000000000 ) ) ;
#14506 = ORIENTED_EDGE ( 'NONE', *, *, #11965, .F. ) ;
#14507 = EDGE_LOOP ( 'NONE', ( #7864, #4229 ) ) ;
#14508 = CARTESIAN_POINT ( 'NONE',  ( 0.1323408341374887331, 6.250000000000000888, 32.00000000000000000 ) ) ;
#14509 = DIRECTION ( 'NONE',  ( 0.000000000000000000, 0.000000000000000000, 1.000000000000000000 ) ) ;
#14510 = CARTESIAN_POINT ( 'NONE',  ( 2.500000000000000000, 3.061616997868383141E-16, 1.400000002184949910 ) ) ;
#14511 = CARTESIAN_POINT ( 'NONE',  ( -2.066987299999999639, 0.000000000000000000, 2.250000001092474999 ) ) ;
#14512 = DIRECTION ( 'NONE',  ( 0.5877852522924802425, -0.8090169943749422332, 0.000000000000000000 ) ) ;
#14513 = CARTESIAN_POINT ( 'NONE',  ( -4.286401442266578599, -4.198423832313146420, 11.49999999999998224 ) ) ;
#14514 = LINE ( 'NONE', #4660, #9543 ) ;
#14515 = CARTESIAN_POINT ( 'NONE',  ( 5.935543223013849179, 0.8771126767607271280, 31.00000000000000000 ) ) ;
#14516 = DIRECTION ( 'NONE',  ( -0.3090169943749584980, 0.9510565162951498674, 0.000000000000000000 ) ) ;
#14517 = DIRECTION ( 'NONE',  ( 0.000000000000000000, 1.000000000000000000, 0.000000000000000000 ) ) ;
#14518 = PRODUCT_DEFINITION_SHAPE ( 'NONE', 'NONE',  #6346 ) ;
#14519 = CARTESIAN_POINT ( 'NONE',  ( -2.500000000000000444, 187.4999999978150527, 7.000000000000000000 ) ) ;
#14520 = CARTESIAN_POINT ( 'NONE',  ( 0.3927937339364459546, 226.3329534510998542, 4.509583726312986762 ) ) ;
#14521 = CARTESIAN_POINT ( 'NONE',  ( 5.770288754215171956, -2.404361317819854182, 17.12618035954928075 ) ) ;
#14522 = CARTESIAN_POINT ( 'NONE',  ( 5.747343991580175171, 1.727858744772314159, 31.99992002356261267 ) ) ;
#14523 = EDGE_LOOP ( 'NONE', ( #1833, #3889 ) ) ;
#14524 = CARTESIAN_POINT ( 'NONE',  ( -3.634089073485431420, 4.776071126502690944, 4.000079976437387330 ) ) ;
#14525 = CARTESIAN_POINT ( 'NONE',  ( -0.8738118504724939895, -5.936246475285042123, 12.00357242174242423 ) ) ;
#14527 = EDGE_LOOP ( 'NONE', ( #10205, #12017 ) ) ;
#14526 = CARTESIAN_POINT ( 'NONE',  ( 5.931793676715113151, 0.9035324301687462922, 24.76239891805597537 ) ) ;
#14528 = DIRECTION ( 'NONE',  ( 0.000000000000000000, 0.000000000000000000, 1.000000000000000000 ) ) ;
#14529 = LINE ( 'NONE', #9690, #15533 ) ;
#14530 = ORIENTED_EDGE ( 'NONE', *, *, #12350, .F. ) ;
#14531 = DIRECTION ( 'NONE',  ( 0.000000000000000000, -2.775557561562887900E-16, 1.000000000000000000 ) ) ;
#14532 = CARTESIAN_POINT ( 'NONE',  ( 1.461580736456472573, 1.461580736456472795, -0.4499999989075252338 ) ) ;
#14533 = CARTESIAN_POINT ( 'NONE',  ( 5.317509234263970264, -2.779225709350972906, 4.867639214160894845 ) ) ;
#14534 = DIRECTION ( 'NONE',  ( 0.000000000000000000, 0.000000000000000000, 1.000000000000000000 ) ) ;
#14535 = CARTESIAN_POINT ( 'NONE',  ( -6.081509788407740480, 1.446521464462707129, 12.37381964045070504 ) ) ;
#14536 =( BOUNDED_CURVE ( )  B_SPLINE_CURVE ( 2, ( #10140, #14992, #503, #5446, #14833, #6643, #5370, #8954, #6719 ),
 .UNSPECIFIED., .F., .F. ) 
 B_SPLINE_CURVE_WITH_KNOTS ( ( 3, 2, 2, 2, 3 ),
 ( 0.7857142857142856984, 0.8035714285714286031, 0.8214285714285713969, 0.8392857142857143016, 0.8571428571428570953 ),
 .UNSPECIFIED. ) 
 CURVE ( )  GEOMETRIC_REPRESENTATION_ITEM ( )  RATIONAL_B_SPLINE_CURVE ( ( 1.000000000000000000, 0.9238795325112867385, 1.000000000000000000, 0.9238795325112867385, 1.000000000000000000, 0.9238795325112867385, 1.000000000000000000, 0.9238795325112867385, 1.000000000000000000 ) ) 
 REPRESENTATION_ITEM ( '' )  );
#14537 = CARTESIAN_POINT ( 'NONE',  ( 1.035533905932737753, 188.8800000002185016, 4.500000000000000888 ) ) ;
#14538 = CYLINDRICAL_SURFACE ( 'NONE', #6287, 1.000000000000000888 ) ;
#14539 = CARTESIAN_POINT ( 'NONE',  ( -5.940390500375673177, 6.474944468551537824, 31.00000000000000000 ) ) ;
#14540 = CARTESIAN_POINT ( 'NONE',  ( -2.066987299999999639, 0.8561741729129455081, -0.9999999989075253337 ) ) ;
#14541 = CIRCLE ( 'NONE', #8717, 2.499999999999999556 ) ;
#14542 = CARTESIAN_POINT ( 'NONE',  ( 5.616089948629745976, 2.743103014345511070, 17.49563030319846746 ) ) ;
#14543 = VERTEX_POINT ( 'NONE', #11849 ) ;
#14544 = CARTESIAN_POINT ( 'NONE',  ( 0.8561741729129456191, 187.5999999989074922, 4.933012699999999029 ) ) ;
#14545 = CARTESIAN_POINT ( 'NONE',  ( 5.082197683525802034E-17, 185.2499999989074979, 4.933012699999999029 ) ) ;
#14546 = CARTESIAN_POINT ( 'NONE',  ( -4.416678568553683348, -4.422441866694277302, 11.76236973443872280 ) ) ;
#14547 = EDGE_LOOP ( 'NONE', ( #7657, #5281, #7100, #9539, #1192, #5823 ) ) ;
#14548 = ADVANCED_FACE ( 'NONE', ( #8133 ), #962, .F. ) ;
#14549 = DIRECTION ( 'NONE',  ( 0.02819803676014390886, 0.000000000000000000, -0.9996023563011813273 ) ) ;
#14550 = CARTESIAN_POINT ( 'NONE',  ( 5.746619684944276329, -1.730157667110832298, 6.000049320733125136 ) ) ;
#14551 = AXIS2_PLACEMENT_3D ( 'NONE', #5700, #756, #6897 ) ;
#14552 = FACE_OUTER_BOUND ( 'NONE', #15003, .T. ) ;
#14553 = CARTESIAN_POINT ( 'NONE',  ( 7.347881158177969135E-16, 6.250000000000000888, 4.000000000000004441 ) ) ;
#14554 = CARTESIAN_POINT ( 'NONE',  ( 1.461580736456473240, 188.3499999989074922, 5.538419263543526760 ) ) ;
#14555 = LINE ( 'NONE', #9792, #3357 ) ;
#14556 = CARTESIAN_POINT ( 'NONE',  ( 1.035533905932737531, 2.500000000000000444, -2.449999997815050179 ) ) ;
#14557 = CARTESIAN_POINT ( 'NONE',  ( 2.999999999999999556, 1.732050807568877859, -5.500000000000000000 ) ) ;
#14558 = CARTESIAN_POINT ( 'NONE',  ( 5.931793676715104269, -0.9035324301687984727, 11.23760108194400864 ) ) ;
#14559 = CARTESIAN_POINT ( 'NONE',  ( 1.530808498934191916E-15, 22.00000000000000000, -12.50000000000000355 ) ) ;
#14560 = DIRECTION ( 'NONE',  ( -0.000000000000000000, 1.000000000000000000, -0.000000000000000000 ) ) ;
#14561 = CARTESIAN_POINT ( 'NONE',  ( -5.531623157106185573, 2.327208526676387557, 30.12635295315577366 ) ) ;
#14562 = ADVANCED_FACE ( 'NONE', ( #3821 ), #13679, .T. ) ;
#14563 = ORIENTED_EDGE ( 'NONE', *, *, #11067, .F. ) ;
#14564 = VECTOR ( 'NONE', #1422, 1000.000000000000000 ) ;
#14565 = ORIENTED_EDGE ( 'NONE', *, *, #2448, .F. ) ;
#14566 = EDGE_CURVE ( 'NONE', #5961, #8844, #2755, .T. ) ;
#14567 = ORIENTED_EDGE ( 'NONE', *, *, #10914, .F. ) ;
#14568 = CARTESIAN_POINT ( 'NONE',  ( -5.317509234263835260, -2.779225709351231366, 24.49999999999999289 ) ) ;
#14569 = EDGE_LOOP ( 'NONE', ( #13031, #15432, #3587, #7411 ) ) ;
#14570 = CARTESIAN_POINT ( 'NONE',  ( 2.066987299999999639, 0.8561741729129456191, 0.9000000010924746885 ) ) ;
#14571 = CARTESIAN_POINT ( 'NONE',  ( 0.7988914244718127167, 5.947301735519285870, 4.384562891686175412 ) ) ;
#14572 = CARTESIAN_POINT ( 'NONE',  ( -2.500000000000000000, 0.000000000000000000, 0.09999999999999982514 ) ) ;
#14573 = CARTESIAN_POINT ( 'NONE',  ( -2.066987300000000083, 187.2499999989075263, 7.000000000000000000 ) ) ;
#14574 = CIRCLE ( 'NONE', #9004, 12.50000000000000355 ) ;
#14575 = CARTESIAN_POINT ( 'NONE',  ( 1.035533905932739085, -2.500000000000000000, -2.043000000021849782 ) ) ;
#14576 = CARTESIAN_POINT ( 'NONE',  ( 3.673940397442060854E-16, 184.0000000000000000, 3.000000000000000888 ) ) ;
#14577 = CARTESIAN_POINT ( 'NONE',  ( 3.106366801612054029, -5.134708448381249291, 31.87303779027051576 ) ) ;
#14578 = CARTESIAN_POINT ( 'NONE',  ( -0.8561741729129455081, 2.066987299999999639, -2.099999998907525089 ) ) ;
#14579 = ADVANCED_FACE ( 'NONE', ( #7413, #14810, #2791, #12255, #14653, #13453 ), #11220, .T. ) ;
#14580 = DIRECTION ( 'NONE',  ( -0.000000000000000000, 1.000000000000000000, -0.000000000000000000 ) ) ;
#14581 = CARTESIAN_POINT ( 'NONE',  ( -2.381136272098726803, 226.7019369474745361, 5.597090573316407358 ) ) ;
#14582 = B_SPLINE_CURVE_WITH_KNOTS ( 'NONE', 3,
 ( #11744, #13976, #5865, #2188, #9141, #13091, #11667, #9365, #1877, #14049, #5634, #7059, #13013, #12853, #11894, #7930, #6752, #11586 ),
 .UNSPECIFIED., .F., .F.,
 ( 4, 2, 2, 2, 2, 2, 2, 2, 4 ),
 ( 0.003131923598877004410, 0.003523316383094321751, 0.003914709167311639093, 0.004306101951528956001, 0.004697494735746272909, 0.005088887519963589817, 0.005480280304180906725, 0.005871673088398223633, 0.006263065872615540541 ),
 .UNSPECIFIED. ) ;
#14583 = DIRECTION ( 'NONE',  ( 0.000000000000000000, 0.000000000000000000, -1.000000000000000000 ) ) ;
#14584 = ORIENTED_EDGE ( 'NONE', *, *, #10283, .T. ) ;
#14585 = ORIENTED_EDGE ( 'NONE', *, *, #7801, .T. ) ;
#14586 = ORIENTED_EDGE ( 'NONE', *, *, #11076, .T. ) ;
#14587 = EDGE_LOOP ( 'NONE', ( #4395, #2627 ) ) ;
#14588 = CARTESIAN_POINT ( 'NONE',  ( -5.725684683139601105, -2.507514573674792135, 30.20112161576661691 ) ) ;
#14589 = CARTESIAN_POINT ( 'NONE',  ( 3.312524433819772351, -5.004191858254007030, 17.02591947216898660 ) ) ;
#14590 = CARTESIAN_POINT ( 'NONE',  ( 2.500000000000000444, 185.5500000000000114, 8.035533905932739529 ) ) ;
#14591 = ADVANCED_FACE ( 'NONE', ( #3895 ), #12487, .F. ) ;
#14592 = B_SPLINE_CURVE_WITH_KNOTS ( 'NONE', 3,
 ( #9016, #484, #15127, #4304, #13477, #11458, #4223, #6255, #404, #7886, #1673, #1380, #5353, #10199, #12654, #13921, #12727, #871 ),
 .UNSPECIFIED., .F., .F.,
 ( 4, 2, 2, 2, 2, 2, 2, 2, 4 ),
 ( 0.000000000000000000, 0.0003914357524127483529, 0.0007828715048254967059, 0.001174307257238245113, 0.001565743009650993412, 0.001957178762063741927, 0.002348614514476490226, 0.002740050266889238525, 0.003131486019301986824 ),
 .UNSPECIFIED. ) ;
#14593 = CARTESIAN_POINT ( 'NONE',  ( -5.725684683139636633, 2.507514573674706426, 31.79887838423339019 ) ) ;
#14594 = AXIS2_PLACEMENT_3D ( 'NONE', #15091, #2760, #7768 ) ;
#14595 = UNCERTAINTY_MEASURE_WITH_UNIT (LENGTH_MEASURE( 1.000000000000000082E-05 ), #4204, 'distance_accuracy_value', 'NONE');
#14596 = DIRECTION ( 'NONE',  ( -6.123233995736766036E-17, 1.000000000000000000, 0.000000000000000000 ) ) ;
#14597 = PRODUCT_DEFINITION ( 'UNKNOWN', '', #3234, #1793 ) ;
#14598 = CARTESIAN_POINT ( 'NONE',  ( 0.000000000000000000, 2.000000000000000000, 0.000000000000000000 ) ) ;
#14599 = CARTESIAN_POINT ( 'NONE',  ( -4.154121946520968223, 4.670585111242886001, 10.70112161576659915 ) ) ;
#14600 = EDGE_CURVE ( 'NONE', #3437, #12110, #14734, .T. ) ;
#14601 = CARTESIAN_POINT ( 'NONE',  ( -6.155854678529437685, -1.081900940642313236, 23.99574050496988065 ) ) ;
#14602 = CARTESIAN_POINT ( 'NONE',  ( -0.05144838531732269515, 189.9979265964238948, 9.435094243585153251 ) ) ;
#14603 = CARTESIAN_POINT ( 'NONE',  ( 0.000000000000000000, 62.00000000000000000, 0.000000000000000000 ) ) ;
#14604 = CARTESIAN_POINT ( 'NONE',  ( -2.500000000000000888, 189.1499999978150868, 8.035533905932737753 ) ) ;
#14605 = CARTESIAN_POINT ( 'NONE',  ( 1.501755279530002651, 226.4544816774725575, 4.867834892302488115 ) ) ;
#14606 = CARTESIAN_POINT ( 'NONE',  ( 0.8499999999999896527, 7.325252813983392336E-16, -2.649388036945189207 ) ) ;
#14607 = VECTOR ( 'NONE', #11194, 1000.000000000000000 ) ;
#14608 = CARTESIAN_POINT ( 'NONE',  ( -0.9261565315117185060, 190.0733590023996555, 4.344097979414469179 ) ) ;
#14609 = ORIENTED_EDGE ( 'NONE', *, *, #1432, .T. ) ;
#14610 = CARTESIAN_POINT ( 'NONE',  ( -2.668367453516708565, 5.373994336898094026, 5.000000000000004441 ) ) ;
#14611 = CARTESIAN_POINT ( 'NONE',  ( 8.250000000000003553, -1.019131563299854308E-13, 2.000000000000001776 ) ) ;
#14612 = CARTESIAN_POINT ( 'NONE',  ( 5.375913338529152874, 2.664979843780314273, 25.00428920362019980 ) ) ;
#14613 = CARTESIAN_POINT ( 'NONE',  ( 3.458623254138780911, -5.207221900902773370, 31.97377282875268989 ) ) ;
#14614 = CYLINDRICAL_SURFACE ( 'NONE', #12480, 1.000000000000000666 ) ;
#14615 = EDGE_CURVE ( 'NONE', #902, #2089, #4643, .T. ) ;
#14616 = CARTESIAN_POINT ( 'NONE',  ( -2.692693252389644520, 5.362085866495079678, 11.23617396794405465 ) ) ;
#14617 = B_SPLINE_CURVE_WITH_KNOTS ( 'NONE', 3,
 ( #4765, #10962, #9703, #14542, #13345, #9538, #15664, #1328, #12228, #3639, #8514, #7461, #5960, #10727, #8668, #6202, #14375, #7312 ),
 .UNSPECIFIED., .F., .F.,
 ( 4, 2, 2, 2, 2, 2, 2, 2, 4 ),
 ( 0.000000000000000000, 0.0003914357524127464556, 0.0007828715048254929112, 0.001174307257238239258, 0.001565743009650985822, 0.001957178762063732386, 0.002348614514476478517, 0.002740050266889225081, 0.003131486019301971645 ),
 .UNSPECIFIED. ) ;
#14618 = VECTOR ( 'NONE', #182, 1000.000000000000000 ) ;
#14619 = CARTESIAN_POINT ( 'NONE',  ( -1.461580736456472795, 1.461580736456472795, 1.350000001092474644 ) ) ;
#14620 = DIRECTION ( 'NONE',  ( -0.000000000000000000, 1.000000000000000000, -0.000000000000000000 ) ) ;
#14621 =( NAMED_UNIT ( * ) SI_UNIT ( $, .STERADIAN. ) SOLID_ANGLE_UNIT ( ) );
#14622 = DIRECTION ( 'NONE',  ( -1.000000000000000000, 0.000000000000000000, 0.000000000000000000 ) ) ;
#14623 = CARTESIAN_POINT ( 'NONE',  ( 2.500000000000000000, 188.6800000002185129, 8.035533905932739529 ) ) ;
#14624 = FACE_BOUND ( 'NONE', #5025, .T. ) ;
#14625 = CARTESIAN_POINT ( 'NONE',  ( 1.924362066950147332, 228.0923243445923276, 6.506028829785237555 ) ) ;
#14626 = CARTESIAN_POINT ( 'NONE',  ( -1.461580736456472351, -1.461580736456473018, 1.550000001092474822 ) ) ;
#14627 = CARTESIAN_POINT ( 'NONE',  ( 5.649053410273161546, -2.675685104943071213, 25.11517780375841724 ) ) ;
#14628 = EDGE_LOOP ( 'NONE', ( #3503, #6753 ) ) ;
#14629 = CARTESIAN_POINT ( 'NONE',  ( -2.066987300000000971, 186.9999999989074979, 6.143825827087054492 ) ) ;
#14630 = CARTESIAN_POINT ( 'NONE',  ( 0.8561741729129456191, 187.5999999989074922, 4.933012699999999029 ) ) ;
#14631 = CARTESIAN_POINT ( 'NONE',  ( -3.000000000000000444, -1.732050807568878081, -2.500000000000000000 ) ) ;
#14632 = CIRCLE ( 'NONE', #7763, 2.500000000000000444 ) ;
#14634 = ORIENTED_EDGE ( 'NONE', *, *, #7181, .T. ) ;
#14633 = CARTESIAN_POINT ( 'NONE',  ( 1.461580736456473018, 185.3499999989075206, 5.538419263543527649 ) ) ;
#14635 = B_SPLINE_CURVE_WITH_KNOTS ( 'NONE', 3,
 ( #10892, #8598, #5885, #2537, #12232, #1333, #4030, #6206, #1021, #11043, #15590, #9542, #14380, #8356, #2289, #5965, #10809, #4770 ),
 .UNSPECIFIED., .F., .F.,
 ( 4, 2, 2, 2, 2, 2, 2, 2, 4 ),
 ( 0.000000000000000000, 0.0003914898357794970073, 0.0007829796715589940146, 0.001174469507338491130, 0.001565959343117988029, 0.001957449178897484928, 0.002348939014676982261, 0.002740428850456479160, 0.003131918686235976058 ),
 .UNSPECIFIED. ) ;
#14636 = CYLINDRICAL_SURFACE ( 'NONE', #8402, 2.500000000000000000 ) ;
#14637 =( REPRESENTATION_RELATIONSHIP ('NONE','NONE', #11191, #4596 ) REPRESENTATION_RELATIONSHIP_WITH_TRANSFORMATION ( #19 )SHAPE_REPRESENTATION_RELATIONSHIP( ) );
#14638 = CARTESIAN_POINT ( 'NONE',  ( 2.030576276931546336E-13, -6.250000000000000888, 25.49999999999999645 ) ) ;
#14639 = CARTESIAN_POINT ( 'NONE',  ( 5.999999999999999112, 194.5935680195190116, 12.11154058223188379 ) ) ;
#14640 = CARTESIAN_POINT ( 'NONE',  ( -0.9999171162589062245, -6.169494774098559731, 11.36722320330676084 ) ) ;
#14641 = DIRECTION ( 'NONE',  ( 0.000000000000000000, 0.000000000000000000, 1.000000000000000000 ) ) ;
#14642 = CARTESIAN_POINT ( 'NONE',  ( 0.1286560605739063556, 189.6973959400375520, 10.39407231488526762 ) ) ;
#14643 = DIRECTION ( 'NONE',  ( 1.000000000000000000, 0.000000000000000000, 0.000000000000000000 ) ) ;
#14644 = CIRCLE ( 'NONE', #6774, 1.500000000000000000 ) ;
#14645 = DIRECTION ( 'NONE',  ( 0.000000000000000000, 0.000000000000000000, 1.000000000000000000 ) ) ;
#14646 = CARTESIAN_POINT ( 'NONE',  ( -0.2637975869346481095, -6.245592211692898132, 18.97332839949189776 ) ) ;
#14647 = DIRECTION ( 'NONE',  ( 0.000000000000000000, 0.000000000000000000, 1.000000000000000000 ) ) ;
#14648 = CARTESIAN_POINT ( 'NONE',  ( 3.010624175977807848, 5.190832888732320072, 23.70111757752058423 ) ) ;
#14649 = EDGE_CURVE ( 'NONE', #5163, #9339, #14288, .T. ) ;
#14650 = VERTEX_POINT ( 'NONE', #4954 ) ;
#14651 = ORIENTED_EDGE ( 'NONE', *, *, #8176, .T. ) ;
#14652 = ORIENTED_EDGE ( 'NONE', *, *, #11475, .F. ) ;
#14653 = FACE_BOUND ( 'NONE', #3974, .T. ) ;
#14654 = AXIS2_PLACEMENT_3D ( 'NONE', #8188, #13025, #5413 ) ;
#14655 = VERTEX_POINT ( 'NONE', #9804 ) ;
#14656 = CARTESIAN_POINT ( 'NONE',  ( 1.461580736456473018, -1.461580736456472573, 0.7500000010924746663 ) ) ;
#14657 = CARTESIAN_POINT ( 'NONE',  ( 0.000000000000000000, 0.000000000000000000, 5.000000000000004441 ) ) ;
#14658 = CARTESIAN_POINT ( 'NONE',  ( 1.767766952966368654, 1.767766952966369098, -0.2000000000000000944 ) ) ;
#14659 = CARTESIAN_POINT ( 'NONE',  ( -2.066987300000000971, 187.2999999989075661, 7.856174172912944620 ) ) ;
#14660 = CARTESIAN_POINT ( 'NONE',  ( -2.500000000000000000, -1.035533905932739307, 0.9499999999999999556 ) ) ;
#14661 = DIRECTION ( 'NONE',  ( 0.000000000000000000, 0.000000000000000000, 1.000000000000000000 ) ) ;
#14662 = ADVANCED_FACE ( 'NONE', ( #11528 ), #5499, .F. ) ;
#14663 = CARTESIAN_POINT ( 'NONE',  ( 2.782156709077468815, -5.316215864844020977, 31.50312048902376816 ) ) ;
#14664 = CARTESIAN_POINT ( 'NONE',  ( -0.8561741729129455081, 2.066987299999999639, 1.300000001092474822 ) ) ;
#14665 = CARTESIAN_POINT ( 'NONE',  ( 4.153663429050834743, -4.670992970568328850, 4.200668510924230326 ) ) ;
#14666 = CARTESIAN_POINT ( 'NONE',  ( -2.999982576790682476, 227.2579145021288696, 7.234552515775640735 ) ) ;
#14667 = ADVANCED_FACE ( 'NONE', ( #6539 ), #1743, .F. ) ;
#14668 = FACE_OUTER_BOUND ( 'NONE', #12854, .T. ) ;
#14669 = ORIENTED_EDGE ( 'NONE', *, *, #178, .T. ) ;
#14670 = ORIENTED_EDGE ( 'NONE', *, *, #9992, .F. ) ;
#14671 = ORIENTED_EDGE ( 'NONE', *, *, #12116, .F. ) ;
#14672 = CARTESIAN_POINT ( 'NONE',  ( -5.648794263291724960, -2.676232015153657606, 10.88558052754513383 ) ) ;
#14673 = CARTESIAN_POINT ( 'NONE',  ( 0.000000000000000000, 189.6977690162252657, 10.38967773564543862 ) ) ;
#14674 = CARTESIAN_POINT ( 'NONE',  ( -0.8730424326980914529, -5.936362132114464174, 4.495006902185641806 ) ) ;
#14675 = CARTESIAN_POINT ( 'NONE',  ( -5.859221468178962056, -2.178708437343193971, 31.97408542334170889 ) ) ;
#14676 = AXIS2_PLACEMENT_3D ( 'NONE', #5051, #4898, #4817 ) ;
#14677 = FACE_OUTER_BOUND ( 'NONE', #3757, .T. ) ;
#14678 = CARTESIAN_POINT ( 'NONE',  ( 2.500000000000000000, 3.061616997868383141E-16, 2.500000000000000000 ) ) ;
#14679 = DIRECTION ( 'NONE',  ( 0.000000000000000000, 0.000000000000000000, 1.000000000000000000 ) ) ;
#14680 = CARTESIAN_POINT ( 'NONE',  ( 1.035533905932737531, 2.500000000000000444, 2.250000000000000888 ) ) ;
#14681 = CYLINDRICAL_SURFACE ( 'NONE', #2094, 1.000000000000000666 ) ;
#14682 = DIRECTION ( 'NONE',  ( 1.000000000000000000, 0.000000000000000000, 0.000000000000000000 ) ) ;
#14683 = CARTESIAN_POINT ( 'NONE',  ( 1.035533905932738197, 189.3499999978150754, 9.500000000000003553 ) ) ;
#14684 = CARTESIAN_POINT ( 'NONE',  ( 2.383228694455616914, 226.7027912316577556, 5.599607710487992662 ) ) ;
#14685 = DIRECTION ( 'NONE',  ( 1.062480551894329776E-17, 2.775557561562888393E-16, -1.000000000000000000 ) ) ;
#14686 = CARTESIAN_POINT ( 'NONE',  ( -2.909494418114037195, 189.9181870229658671, 6.441359701375095170 ) ) ;
#14687 = ORIENTED_EDGE ( 'NONE', *, *, #9426, .F. ) ;
#14688 = CARTESIAN_POINT ( 'NONE',  ( -3.922672396097064418, 4.541739265057694652, 5.873647046844240549 ) ) ;
#14689 = DIRECTION ( 'NONE',  ( 0.000000000000000000, 0.000000000000000000, 1.000000000000000000 ) ) ;
#14690 = EDGE_CURVE ( 'NONE', #5418, #7973, #1665, .T. ) ;
#14691 = CARTESIAN_POINT ( 'NONE',  ( 13.50000000000000000, -0.001000000000000132727, -8.673617379884035472E-16 ) ) ;
#14692 = CARTESIAN_POINT ( 'NONE',  ( 1.991469598915552641, 226.5678560613478680, 5.201980668966470489 ) ) ;
#14693 = VECTOR ( 'NONE', #13349, 1000.000000000000000 ) ;
#14694 = DIRECTION ( 'NONE',  ( 0.000000000000000000, 1.000000000000000000, 0.000000000000000000 ) ) ;
#14695 = ADVANCED_FACE ( 'NONE', ( #6619 ), #3386, .F. ) ;
#14696 = CARTESIAN_POINT ( 'NONE',  ( 0.8561741729129463963, -2.066987299999999195, 0.1000000010924748939 ) ) ;
#14697 = DIRECTION ( 'NONE',  ( -0.9510565162951545304, 0.3090169943749447867, 0.000000000000000000 ) ) ;
#14698 = PRESENTATION_STYLE_ASSIGNMENT (( #13419 ) ) ;
#14699 = CYLINDRICAL_SURFACE ( 'NONE', #1881, 2.500000000000000444 ) ;
#14700 = CARTESIAN_POINT ( 'NONE',  ( -1.767766952966369098, 184.2999999999999829, 5.232233047033630235 ) ) ;
#14701 = CARTESIAN_POINT ( 'NONE',  ( -4.286401442266578599, -4.198423832313146420, 11.49999999999998224 ) ) ;
#14702 = CARTESIAN_POINT ( 'NONE',  ( 1.618192118698865700, 228.6399984490590214, 8.087742880769061671 ) ) ;
#14703 = CARTESIAN_POINT ( 'NONE',  ( -1.461580736456472351, -1.461580736456473018, -2.449999998907525178 ) ) ;
#14704 = ADVANCED_FACE ( 'NONE', ( #15120 ), #626, .F. ) ;
#14705 = CARTESIAN_POINT ( 'NONE',  ( 0.2638277032949121748, 5.995407492418038053, 31.97332055281518137 ) ) ;
#14706 = B_SPLINE_CURVE_WITH_KNOTS ( 'NONE', 3,
 ( #7120, #9750, #14257, #5926, #11871, #14588, #13386, #5845, #1062, #10847, #8561, #11956, #8235, #14423, #3529, #15710, #8399, #10772 ),
 .UNSPECIFIED., .F., .F.,
 ( 4, 2, 2, 2, 2, 2, 2, 2, 4 ),
 ( 0.003131486019301978150, 0.003522824630466686157, 0.003914163241631393730, 0.004305501852796101737, 0.004696840463960809745, 0.005088179075125517752, 0.005479517686290225759, 0.005870856297454933766, 0.006262194908619641773 ),
 .UNSPECIFIED. ) ;
#14707 = EDGE_LOOP ( 'NONE', ( #14652, #13217, #4970, #9862 ) ) ;
#14708 = CARTESIAN_POINT ( 'NONE',  ( -1.265664690411614835E-16, 2.066987299999999639, 1.050000001092474822 ) ) ;
#14709 = AXIS2_PLACEMENT_3D ( 'NONE', #1310, #8500, #2517 ) ;
#14710 = CARTESIAN_POINT ( 'NONE',  ( -0.8561741729129457301, 186.8999999989075036, 4.933012699999999029 ) ) ;
#14711 = CYLINDRICAL_SURFACE ( 'NONE', #7830, 1.000000000000000666 ) ;
#14712 = CIRCLE ( 'NONE', #6836, 2.499999999999999556 ) ;
#14714 = ORIENTED_EDGE ( 'NONE', *, *, #9426, .T. ) ;
#14713 = CARTESIAN_POINT ( 'NONE',  ( 4.344265632482096073, 4.493596842504949507, 30.49574050496988420 ) ) ;
#14715 = CARTESIAN_POINT ( 'NONE',  ( -4.286401442266677186, -4.198423832313046944, 24.36935038651144225 ) ) ;
#14716 = CARTESIAN_POINT ( 'NONE',  ( 0.1323736289506388109, -6.249999999999996447, 25.49999999999999645 ) ) ;
#14717 = CARTESIAN_POINT ( 'NONE',  ( 2.817313151350923750, 5.579000502529566141, 24.63063932754212004 ) ) ;
#14718 = CARTESIAN_POINT ( 'NONE',  ( 5.999999999999999112, 187.9952603975225429, 3.440894205938198613 ) ) ;
#14719 = CARTESIAN_POINT ( 'NONE',  ( -1.768703179866833342, 189.0000639513403939, 5.233169770031948609 ) ) ;
#14720 = AXIS2_PLACEMENT_3D ( 'NONE', #12815, #3198, #5442 ) ;
#14721 = FACE_BOUND ( 'NONE', #7277, .T. ) ;
#14722 = CARTESIAN_POINT ( 'NONE',  ( 0.000000000000000000, 2.000000000000000000, -13.50000000000000000 ) ) ;
#14723 = CIRCLE ( 'NONE', #4297, 1.499999999999999556 ) ;
#14724 = DIRECTION ( 'NONE',  ( -1.000000000000000000, 0.000000000000000000, 0.000000000000000000 ) ) ;
#14725 = AXIS2_PLACEMENT_3D ( 'NONE', #2566, #12345, #5278 ) ;
#14726 = CARTESIAN_POINT ( 'NONE',  ( 11.25000000000000355, -1.020968533498575335E-13, 0.000000000000000000 ) ) ;
#14727 = CARTESIAN_POINT ( 'NONE',  ( -2.817313151351207523, 5.579000502529421368, 30.86765874365831763 ) ) ;
#14728 = DIRECTION ( 'NONE',  ( 0.5877852522924802425, -0.8090169943749422332, 0.000000000000000000 ) ) ;
#14729 = CARTESIAN_POINT ( 'NONE',  ( 3.311576095066412151, 5.004818610361416731, 23.52622176056705783 ) ) ;
#14730 = EDGE_LOOP ( 'NONE', ( #7199, #1957 ) ) ;
#14731 = EDGE_LOOP ( 'NONE', ( #1723, #3545 ) ) ;
#14732 = AXIS2_PLACEMENT_3D ( 'NONE', #9072, #14950, #4041 ) ;
#14733 = VERTEX_POINT ( 'NONE', #12721 ) ;
#14734 = LINE ( 'NONE', #13527, #12910 ) ;
#14735 = EDGE_LOOP ( 'NONE', ( #1403, #8254, #2871, #7334 ) ) ;
#14736 = CARTESIAN_POINT ( 'NONE',  ( -2.066987299999999639, 0.8561741729129452860, -0.3999999989075250784 ) ) ;
#14737 = CARTESIAN_POINT ( 'NONE',  ( 5.571002711501436444, 2.833546409886228190, 18.26379616840806008 ) ) ;
#14738 = CARTESIAN_POINT ( 'NONE',  ( 0.000000000000000000, 0.000000000000000000, 0.000000000000000000 ) ) ;
#14739 = CARTESIAN_POINT ( 'NONE',  ( -0.1323736289504250097, 6.250000000000000000, 25.49999999999997158 ) ) ;
#14740 = CARTESIAN_POINT ( 'NONE',  ( -1.767766952966369098, 1.767766952966369098, 1.599999999999999867 ) ) ;
#14741 = DIRECTION ( 'NONE',  ( 0.000000000000000000, 0.000000000000000000, 1.000000000000000000 ) ) ;
#14742 = ITEM_DEFINED_TRANSFORMATION ( 'NONE', 'NONE', #10861,  #14201 ) ;
#14743 =( GEOMETRIC_REPRESENTATION_CONTEXT ( 3 ) GLOBAL_UNCERTAINTY_ASSIGNED_CONTEXT ( ( #2333 ) ) GLOBAL_UNIT_ASSIGNED_CONTEXT ( ( #8736, #9697, #288 ) ) REPRESENTATION_CONTEXT ( 'NONE', 'WORKASPACE' ) );
#14744 = LINE ( 'NONE', #2564, #13835 ) ;
#14745 = CARTESIAN_POINT ( 'NONE',  ( 1.461580736456472573, 1.461580736456472795, -2.249999998907525001 ) ) ;
#14746 = CARTESIAN_POINT ( 'NONE',  ( -5.859221468178992254, 2.178708437343110482, 30.02591457665829466 ) ) ;
#14747 = CARTESIAN_POINT ( 'NONE',  ( -2.548643141829932901, 227.7997363639018147, 8.829041127271985090 ) ) ;
#14748 = B_SPLINE_CURVE_WITH_KNOTS ( 'NONE', 3,
 ( #11509, #7779, #455, #2691, #2930, #5248, #5403, #7625, #4119, #4037, #8911, #5327, #12390, #2773, #4199, #10251, #11357, #6367 ),
 .UNSPECIFIED., .F., .F.,
 ( 4, 2, 2, 2, 2, 2, 2, 2, 4 ),
 ( 0.000000000000000000, 0.0003914357524127471603, 0.0007828715048254943206, 0.001174307257238241427, 0.001565743009650988641, 0.001957178762063735856, 0.002348614514476482854, 0.002740050266889230285, 0.003131486019301977283 ),
 .UNSPECIFIED. ) ;
#14749 = ORIENTED_EDGE ( 'NONE', *, *, #6913, .F. ) ;
#14750 = ORIENTED_EDGE ( 'NONE', *, *, #9440, .F. ) ;
#14751 = ORIENTED_EDGE ( 'NONE', *, *, #15149, .F. ) ;
#14752 = CARTESIAN_POINT ( 'NONE',  ( 1.000079958708271821, 5.916066267613677709, 18.13152738882034143 ) ) ;
#14753 = CARTESIAN_POINT ( 'NONE',  ( 2.328196544889883590, 189.0000000000000284, 6.072157969751945217 ) ) ;
#14754 = ADVANCED_FACE ( 'NONE', ( #11605, #9160 ), #11374, .T. ) ;
#14755 = CARTESIAN_POINT ( 'NONE',  ( -5.648794263291692097, -2.676232015153728216, 17.38558052754515160 ) ) ;
#14756 = ADVANCED_FACE ( 'NONE', ( #14277 ), #2190, .F. ) ;
#14757 = CARTESIAN_POINT ( 'NONE',  ( 0.6151877315911188360, -6.220340188096003864, 18.79906673469668732 ) ) ;
#14758 = CARTESIAN_POINT ( 'NONE',  ( 0.6156307853270029939, 5.969051238897248979, 12.29870573410680556 ) ) ;
#14759 = CARTESIAN_POINT ( 'NONE',  ( 2.500000000000000444, 186.2999999978150356, 7.000000000000000000 ) ) ;
#14760 = DIRECTION ( 'NONE',  ( 0.000000000000000000, 0.000000000000000000, 1.000000000000000000 ) ) ;
#14761 = CARTESIAN_POINT ( 'NONE',  ( 5.620786884546321360, -2.102685372472797631, 12.47358595436692319 ) ) ;
#14762 = CARTESIAN_POINT ( 'NONE',  ( -2.841041022017514184, 5.567186575787197889, 18.26225281721714566 ) ) ;
#14763 = CARTESIAN_POINT ( 'NONE',  ( 0.000000000000000000, 104.0000000000000142, 0.000000000000000000 ) ) ;
#14764 = CARTESIAN_POINT ( 'NONE',  ( 1.767766952966368432, 187.0699999975965397, 8.767766952966368876 ) ) ;
#14765 = CARTESIAN_POINT ( 'NONE',  ( -0.8231351400649619121, 227.6668932001845462, 5.277359419731677548 ) ) ;
#14766 = CARTESIAN_POINT ( 'NONE',  ( 0.8272382227408706656, 226.3624115040579738, 4.596429122765971265 ) ) ;
#14767 = CARTESIAN_POINT ( 'NONE',  ( -2.495860339748324108, 189.0000000026251712, 6.620890110190097211 ) ) ;
#14768 = ORIENTED_EDGE ( 'NONE', *, *, #358, .F. ) ;
#14769 = CARTESIAN_POINT ( 'NONE',  ( -4.196038884587180995, 4.289036423669260856, 5.503897950159858610 ) ) ;
#14770 = EDGE_CURVE ( 'NONE', #13893, #14222, #3523, .T. ) ;
#14771 = CARTESIAN_POINT ( 'NONE',  ( 3.568242062701560524, -5.132954954975482487, 10.49995093123465217 ) ) ;
#14772 = CARTESIAN_POINT ( 'NONE',  ( 0.1306394121200051550, -6.250000000000003553, 10.49999999999998579 ) ) ;
#14773 = CARTESIAN_POINT ( 'NONE',  ( -0.07717340183324797320, 189.6978550888158281, 10.38866401756451552 ) ) ;
#14774 = CARTESIAN_POINT ( 'NONE',  ( 2.982602392329962715, 227.1840276311630475, 7.016963325779705052 ) ) ;
#14775 = CARTESIAN_POINT ( 'NONE',  ( -2.849573632035303561, 5.280958870664584914, 10.88438267301394369 ) ) ;
#14776 = CARTESIAN_POINT ( 'NONE',  ( 2.500000000000000000, 3.061616997868383141E-16, 2.100000000000000089 ) ) ;
#14777 = CARTESIAN_POINT ( 'NONE',  ( 5.843318061569054755, -1.367618216965598821, 4.126962209729495790 ) ) ;
#14778 = CARTESIAN_POINT ( 'NONE',  ( -0.7988860301921972829, -6.199427171881341181, 30.38455580536194134 ) ) ;
#14779 = CARTESIAN_POINT ( 'NONE',  ( 1.767766952966369320, 184.9000000000000057, 5.232233047033630235 ) ) ;
#14780 = FACE_OUTER_BOUND ( 'NONE', #14441, .T. ) ;
#14781 = CARTESIAN_POINT ( 'NONE',  ( 1.884974866327016940, 228.4701649684375866, 7.597254102066775872 ) ) ;
#14782 = CARTESIAN_POINT ( 'NONE',  ( 2.066987300000000083, -0.8561741729129450640, -2.199999998907525178 ) ) ;
#14783 = CARTESIAN_POINT ( 'NONE',  ( 3.779681992289742887, 4.979315417303941338, 12.49995078984291830 ) ) ;
#14784 = CARTESIAN_POINT ( 'NONE',  ( 2.066987300000000083, -0.8561741729129450640, 1.600000001092474644 ) ) ;
#14785 = VECTOR ( 'NONE', #9427, 1000.000000000000000 ) ;
#14786 = CARTESIAN_POINT ( 'NONE',  ( 2.066987300000000083, 189.0499999989075093, 7.000000000000000000 ) ) ;
#14787 = CARTESIAN_POINT ( 'NONE',  ( 2.500000000000000444, 187.1499999978150584, 5.964466094067262247 ) ) ;
#14789 = EDGE_LOOP ( 'NONE', ( #11486, #2254 ) ) ;
#14788 = CARTESIAN_POINT ( 'NONE',  ( 2.066987300000000083, 186.0999999989075206, 6.143825827087054492 ) ) ;
#14790 = DIRECTION ( 'NONE',  ( 0.000000000000000000, 0.000000000000000000, -1.000000000000000000 ) ) ;
#14791 = CARTESIAN_POINT ( 'NONE',  ( 6.143143148203064285, -1.154591847827665774, 12.11396179408069607 ) ) ;
#14792 = ADVANCED_FACE ( 'NONE', ( #5422 ), #475, .F. ) ;
#14793 = CARTESIAN_POINT ( 'NONE',  ( 4.416779112813619790, -4.422345839825831071, 17.73774718278285079 ) ) ;
#14794 = CARTESIAN_POINT ( 'NONE',  ( -5.999999999999999112, 187.2933328889893403, 9.583808270834989429 ) ) ;
#14795 = CARTESIAN_POINT ( 'NONE',  ( -2.445702039570965436, 189.0000000000000284, 6.417294754563008574 ) ) ;
#14796 = CARTESIAN_POINT ( 'NONE',  ( 2.668367453516506060, 5.373994336898192614, 17.86938304467859950 ) ) ;
#14797 = CIRCLE ( 'NONE', #803, 3.118365096457675012 ) ;
#14798 = CARTESIAN_POINT ( 'NONE',  ( 0.9662756667218489470, 2.500000000000000000, -3.246655914206870275 ) ) ;
#14799 = DIRECTION ( 'NONE',  ( -0.000000000000000000, 1.000000000000000000, -0.000000000000000000 ) ) ;
#14800 = CARTESIAN_POINT ( 'NONE',  ( 2.900815891035680938, 189.8415453012541718, 8.113821064254620907 ) ) ;
#14801 = CARTESIAN_POINT ( 'NONE',  ( -0.5042675786777902625, -6.230788509548851550, 18.87331068310446369 ) ) ;
#14802 = CARTESIAN_POINT ( 'NONE',  ( -5.935543223013839409, -0.8771126767608161678, 11.63239388001634289 ) ) ;
#14803 = CARTESIAN_POINT ( 'NONE',  ( -4.286401442266737583, 4.198423832312984771, 24.49999999999999289 ) ) ;
#14804 = ORIENTED_EDGE ( 'NONE', *, *, #2925, .T. ) ;
#14805 = CARTESIAN_POINT ( 'NONE',  ( 2.066987299999999639, 188.4499999989075150, 7.000000000000000000 ) ) ;
#14806 = ORIENTED_EDGE ( 'NONE', *, *, #9648, .T. ) ;
#14807 = CARTESIAN_POINT ( 'NONE',  ( 7.180990026460783326, -3.384707322287269893, 17.99999999999998934 ) ) ;
#14808 = ORIENTED_EDGE ( 'NONE', *, *, #8456, .F. ) ;
#14809 = AXIS2_PLACEMENT_3D ( 'NONE', #3069, #2993, #12761 ) ;
#14810 = FACE_BOUND ( 'NONE', #12837, .T. ) ;
#14811 = ORIENTED_EDGE ( 'NONE', *, *, #842, .T. ) ;
#14812 = CARTESIAN_POINT ( 'NONE',  ( 0.8561741729129463963, -2.066987299999999195, 0.7000000010924749549 ) ) ;
#14813 = CARTESIAN_POINT ( 'NONE',  ( 5.649200442566199243, 2.675373855294061798, 18.61560192892921251 ) ) ;
#14814 = CARTESIAN_POINT ( 'NONE',  ( -2.367857196298859268, 227.8856709934939317, 9.081849937883657020 ) ) ;
#14815 = DIRECTION ( 'NONE',  ( 0.8090169943749506709, -0.5877852522924689183, 0.000000000000000000 ) ) ;
#14816 = CARTESIAN_POINT ( 'NONE',  ( -1.767766952966368432, -1.767766952966369320, 1.800000000000000044 ) ) ;
#14817 = DIRECTION ( 'NONE',  ( 0.000000000000000000, -1.000000000000000000, 0.000000000000000000 ) ) ;
#14818 = ITEM_DEFINED_TRANSFORMATION ( 'NONE', 'NONE', #15693,  #14201 ) ;
#14819 = CARTESIAN_POINT ( 'NONE',  ( 4.286401442266533302, 4.198423832313197046, 5.132393880016353549 ) ) ;
#14820 = CARTESIAN_POINT ( 'NONE',  ( -0.8561741729129458411, -2.066987299999999195, -0.7999999989075252671 ) ) ;
#14821 = TOROIDAL_SURFACE ( 'NONE', #13019, 2.483389555546409166, 0.1000000000000000056 ) ;
#14822 = CARTESIAN_POINT ( 'NONE',  ( 6.176542424588132185, -0.9554180641284774067, 11.36939309276498911 ) ) ;
#14823 = CARTESIAN_POINT ( 'NONE',  ( -1.978640506925948062, 228.0159251728749155, 9.464911921216582869 ) ) ;
#14824 = ORIENTED_EDGE ( 'NONE', *, *, #1717, .F. ) ;
#14825 = ORIENTED_EDGE ( 'NONE', *, *, #11157, .T. ) ;
#14826 = ORIENTED_EDGE ( 'NONE', *, *, #8880, .T. ) ;
#14827 = FACE_OUTER_BOUND ( 'NONE', #7732, .T. ) ;
#14828 = CARTESIAN_POINT ( 'NONE',  ( 0.7947751898797416059, 188.9999999999999716, 4.622669033327397869 ) ) ;
#14829 = VERTEX_POINT ( 'NONE', #9087 ) ;
#14830 = CARTESIAN_POINT ( 'NONE',  ( -0.9999196734182633772, -5.916093360767516351, 4.867259559550685566 ) ) ;
#14831 = CARTESIAN_POINT ( 'NONE',  ( -2.692693252389637859, -5.362085866495083231, 18.26382603205596311 ) ) ;
#14832 = CARTESIAN_POINT ( 'NONE',  ( -3.000000000000000000, 1.732050807568877415, -2.500000000000000000 ) ) ;
#14833 = CARTESIAN_POINT ( 'NONE',  ( 4.592425496802573972E-16, -2.500000000000000000, -2.100000000000000089 ) ) ;
#14834 = CARTESIAN_POINT ( 'NONE',  ( 2.500000000000000444, 185.5499999978150640, 5.964466094067262247 ) ) ;
#14835 = CARTESIAN_POINT ( 'NONE',  ( -2.817313151351249711, 5.579000502529400940, 11.49999999999998224 ) ) ;
#14836 = CARTESIAN_POINT ( 'NONE',  ( 0.2619456584324066362, -5.995505046955607042, 23.52607193928647433 ) ) ;
#14837 = APPLICATION_PROTOCOL_DEFINITION ( 'draft international standard', 'automotive_design', 1998, #10449 ) ;
#14838 = CARTESIAN_POINT ( 'NONE',  ( 2.500000000000000444, 186.4199999975966193, 5.964466094067262247 ) ) ;
#14839 = CARTESIAN_POINT ( 'NONE',  ( -1.690976820968455474, 227.9165037442230926, 5.998248907768082283 ) ) ;
#14840 = CARTESIAN_POINT ( 'NONE',  ( -3.000008639299222235, 227.3051114066062155, 7.373492455173472848 ) ) ;
#14841 = AXIS2_PLACEMENT_3D ( 'NONE', #6611, #15113, #15035 ) ;
#14842 = EDGE_CURVE ( 'NONE', #6001, #15154, #4136, .T. ) ;
#14843 = CARTESIAN_POINT ( 'NONE',  ( -2.694542719975550948, 189.3631562369849064, 5.701170958452144610 ) ) ;
#14844 = ORIENTED_EDGE ( 'NONE', *, *, #5021, .T. ) ;
#14845 = CARTESIAN_POINT ( 'NONE',  ( 2.000000000000001776, 0.000000000000000000, 0.000000000000000000 ) ) ;
#14846 = CARTESIAN_POINT ( 'NONE',  ( -9.750000000000003553, 184.0000000000000000, -3.401296724241641415E-14 ) ) ;
#14847 = CARTESIAN_POINT ( 'NONE',  ( -3.736532060718149140, 4.696070028785846340, 23.52622176056705783 ) ) ;
#14848 = CARTESIAN_POINT ( 'NONE',  ( 1.000079958708342653, 5.916066267613666163, 24.63152738882033432 ) ) ;
#14849 = CARTESIAN_POINT ( 'NONE',  ( 1.170086215019673359, 228.1786594689324659, 9.943436085668160729 ) ) ;
#14850 = CARTESIAN_POINT ( 'NONE',  ( 3.011899281037336173, -5.190111395030321262, 23.69977782616121331 ) ) ;
#14851 = CARTESIAN_POINT ( 'NONE',  ( 2.500000000000000000, 3.061616997868383141E-16, 1.300000000000000044 ) ) ;
#14852 = CARTESIAN_POINT ( 'NONE',  ( -4.416678568553842332, 4.422441866694120094, 24.23763026556123634 ) ) ;
#14853 = CARTESIAN_POINT ( 'NONE',  ( 5.931793676715082952, 0.9035324301689496851, 5.262398918055979813 ) ) ;
#14854 = CARTESIAN_POINT ( 'NONE',  ( 1.035533905932738197, 187.0499999999999829, 9.500000000000003553 ) ) ;
#14855 = FACE_BOUND ( 'NONE', #4708, .T. ) ;
#14856 = EDGE_CURVE ( 'NONE', #3740, #5609, #4217, .T. ) ;
#14857 = CARTESIAN_POINT ( 'NONE',  ( -0.3251550031287174236, 227.6173728764936186, 5.134341900458684549 ) ) ;
#14858 = CARTESIAN_POINT ( 'NONE',  ( -1.265664690411614835E-16, 2.066987299999999639, -1.149999998907525356 ) ) ;
#14859 = CARTESIAN_POINT ( 'NONE',  ( -3.882673863916255463, -4.899192824800964630, 10.52591457665827512 ) ) ;
#14860 = DIRECTION ( 'NONE',  ( 0.000000000000000000, 2.775557561562887900E-16, -1.000000000000000000 ) ) ;
#14861 = CARTESIAN_POINT ( 'NONE',  ( -1.035533905932737753, 184.2500000000000000, 4.500000000000000888 ) ) ;
#14862 = CARTESIAN_POINT ( 'NONE',  ( -4.005361199355110813, 4.468319061418669413, 18.80022217383877958 ) ) ;
#14863 = ADVANCED_FACE ( 'NONE', ( #2948 ), #7796, .F. ) ;
#14865 = ORIENTED_EDGE ( 'NONE', *, *, #6920, .F. ) ;
#14864 = CARTESIAN_POINT ( 'NONE',  ( -1.461580736456473462, 188.9499999989075150, 8.461580736456472351 ) ) ;
#14866 = DIRECTION ( 'NONE',  ( 1.000000000000000000, 0.000000000000000000, 0.000000000000000000 ) ) ;
#14867 = CARTESIAN_POINT ( 'NONE',  ( 5.770331821586440313, -2.404225004693508527, 12.37380055247394672 ) ) ;
#14868 = CARTESIAN_POINT ( 'NONE',  ( -5.999999999999999112, 188.6555110544239824, 3.692234042171783415 ) ) ;
#14869 = CYLINDRICAL_SURFACE ( 'NONE', #13953, 1.000000000000000222 ) ;
#14870 = CARTESIAN_POINT ( 'NONE',  ( 5.915699123067200027, -1.003533581835301280, 25.00389795015983552 ) ) ;
#14871 = CARTESIAN_POINT ( 'NONE',  ( 1.934702460432737414, 190.0213251105361962, 4.917537802262033964 ) ) ;
#14872 = CARTESIAN_POINT ( 'NONE',  ( 0.08570591359081922156, -0.3999999999999906408, -2.551355435856202281 ) ) ;
#14873 = CARTESIAN_POINT ( 'NONE',  ( 5.531757352715619191, -2.326874507723291963, 10.62619317285287934 ) ) ;
#14874 = CARTESIAN_POINT ( 'NONE',  ( -0.1306070469492023600, -6.250000000000004441, 16.99999999999999289 ) ) ;
#14875 = FACE_OUTER_BOUND ( 'NONE', #4052, .T. ) ;
#14876 = CARTESIAN_POINT ( 'NONE',  ( -7.799024015210663130, -1.482594289697217294, 5.000000000000004441 ) ) ;
#14877 = CIRCLE ( 'NONE', #8790, 1.499999999999999556 ) ;
#14878 = EDGE_LOOP ( 'NONE', ( #11373, #9118 ) ) ;
#14879 = CARTESIAN_POINT ( 'NONE',  ( -2.066987300000000971, 187.2999999989075661, 7.856174172912944620 ) ) ;
#14880 = PRESENTATION_LAYER_ASSIGNMENT (  '', '', ( #8272 ) ) ;
#14881 = ADVANCED_FACE ( 'NONE', ( #3025 ), #1821, .F. ) ;
#14882 = EDGE_LOOP ( 'NONE', ( #5998, #5199 ) ) ;
#14883 = CARTESIAN_POINT ( 'NONE',  ( -5.665308849928751833, -1.980336949702712790, 23.50007997643738022 ) ) ;
#14884 = VERTEX_POINT ( 'NONE', #10423 ) ;
#14885 = CARTESIAN_POINT ( 'NONE',  ( 0.000000000000000000, 0.000000000000000000, 0.000000000000000000 ) ) ;
#14886 = DIRECTION ( 'NONE',  ( -6.123233995736766036E-17, 1.000000000000000000, 0.000000000000000000 ) ) ;
#14887 = VERTEX_POINT ( 'NONE', #15275 ) ;
#14888 = CARTESIAN_POINT ( 'NONE',  ( -1.461580736456472795, 1.461580736456472795, -2.049999998907525711 ) ) ;
#14889 = CIRCLE ( 'NONE', #5738, 3.000000000000000000 ) ;
#14890 = CARTESIAN_POINT ( 'NONE',  ( 0.2638277032948923018, 5.995407492418038053, 5.973320552815183149 ) ) ;
#14891 = CARTESIAN_POINT ( 'NONE',  ( -0.07717340183324797320, 189.6978550888158281, 10.38866401756451552 ) ) ;
#14892 = LINE ( 'NONE', #328, #1327 ) ;
#14893 = CARTESIAN_POINT ( 'NONE',  ( 2.500000000000000000, 3.061616997868383141E-16, 1.300000000000000044 ) ) ;
#14894 = FACE_OUTER_BOUND ( 'NONE', #6228, .T. ) ;
#14895 = CARTESIAN_POINT ( 'NONE',  ( 3.633127580202317741, -4.776802569231024975, 32.00007961174476634 ) ) ;
#14896 = CARTESIAN_POINT ( 'NONE',  ( 1.461580736456473018, -1.461580736456472573, -0.6499999989075253559 ) ) ;
#14897 = CARTESIAN_POINT ( 'NONE',  ( 5.770288754215145310, -2.404361317819922572, 10.62618035954928253 ) ) ;
#14898 = CARTESIAN_POINT ( 'NONE',  ( 3.011899281037413889, 5.190111395030279517, 12.30022217383879024 ) ) ;
#14899 = ORIENTED_EDGE ( 'NONE', *, *, #9799, .F. ) ;
#14900 = EDGE_LOOP ( 'NONE', ( #1354, #15135 ) ) ;
#14901 = EDGE_CURVE ( 'NONE', #9480, #4645, #4375, .T. ) ;
#14902 = ORIENTED_EDGE ( 'NONE', *, *, #14994, .F. ) ;
#14903 = CARTESIAN_POINT ( 'NONE',  ( -2.897581130414634077E-17, 19.99999999999999645, -9.750000000000003553 ) ) ;
#14904 = CARTESIAN_POINT ( 'NONE',  ( 4.435347140101010055, 4.403429997944536822, 5.000000000000004441 ) ) ;
#14905 = EDGE_LOOP ( 'NONE', ( #7795, #9662, #11973, #10030 ) ) ;
#14906 = CARTESIAN_POINT ( 'NONE',  ( -5.558508435838124484, -2.857531096719054808, 17.86939309276500154 ) ) ;
#14907 = CARTESIAN_POINT ( 'NONE',  ( 0.5043776560898699524, -6.230795654995827881, 18.87337476296010053 ) ) ;
#14908 = CARTESIAN_POINT ( 'NONE',  ( -0.2622538972263916968, 6.245673238944478456, 18.97385994369195572 ) ) ;
#14909 = CARTESIAN_POINT ( 'NONE',  ( -2.500000000000000444, 187.5499999978150356, 8.035533905932737753 ) ) ;
#14910 = CARTESIAN_POINT ( 'NONE',  ( -1.767766952966369320, 186.5999999978150754, 5.232233047033630235 ) ) ;
#14911 = CARTESIAN_POINT ( 'NONE',  ( -2.817313151351372724, 5.579000502529338767, 24.49999999999999289 ) ) ;
#14912 = CARTESIAN_POINT ( 'NONE',  ( -4.070863287254184115, 4.743975846881713920, 10.62694108445697161 ) ) ;
#14913 = VECTOR ( 'NONE', #11137, 1000.000000000000000 ) ;
#14914 = CARTESIAN_POINT ( 'NONE',  ( 2.668367453516506504, 5.373994336898192614, 17.99999999999998934 ) ) ;
#14915 = DIRECTION ( 'NONE',  ( 1.000000000000000000, 0.000000000000000000, 0.000000000000000000 ) ) ;
#14916 = CARTESIAN_POINT ( 'NONE',  ( -1.767766952966369320, 187.4699999975965454, 5.232233047033630235 ) ) ;
#14917 = CARTESIAN_POINT ( 'NONE',  ( -1.813734975128623139, 228.5291423394705532, 7.767584113458720019 ) ) ;
#14918 = CARTESIAN_POINT ( 'NONE',  ( -2.809196860006122787, 226.9495188873497966, 6.326437523183426670 ) ) ;
#14919 = CARTESIAN_POINT ( 'NONE',  ( -1.819594887494103475, 189.1119032262050439, 9.571239929234401700 ) ) ;
#14920 = ORIENTED_EDGE ( 'NONE', *, *, #9262, .T. ) ;
#14921 = CARTESIAN_POINT ( 'NONE',  ( -5.866923913994642525, 1.260079467906539241, 12.29952054102714243 ) ) ;
#14922 = VECTOR ( 'NONE', #8089, 1000.000000000000000 ) ;
#14923 = FACE_OUTER_BOUND ( 'NONE', #8068, .T. ) ;
#14924 = CARTESIAN_POINT ( 'NONE',  ( -1.000049271338485646, 6.169473353325552800, 4.869696127045516576 ) ) ;
#14925 = CARTESIAN_POINT ( 'NONE',  ( 13.50000000000000000, 2.000000000000000000, -8.673617379884035472E-16 ) ) ;
#14926 = CARTESIAN_POINT ( 'NONE',  ( 2.839005933515748925, 227.6017802382847037, 8.246656694154813394 ) ) ;
#14927 = CARTESIAN_POINT ( 'NONE',  ( 3.459597053047843040, 5.206576120509745387, 5.974085423341712442 ) ) ;
#14928 = CARTESIAN_POINT ( 'NONE',  ( -1.265664690411614835E-16, 2.066987299999999639, -2.749999998907525001 ) ) ;
#14929 = CARTESIAN_POINT ( 'NONE',  ( 2.692335458626892386, 5.362264153667214650, 4.737601081944043280 ) ) ;
#14930 = ADVANCED_FACE ( 'NONE', ( #3010 ), #12473, .F. ) ;
#14931 = DIRECTION ( 'NONE',  ( -0.9510565162951544194, 0.3090169943749447312, 0.000000000000000000 ) ) ;
#14932 = CARTESIAN_POINT ( 'NONE',  ( 2.500000000000000444, 187.2500000000000000, 5.964466094067262247 ) ) ;
#14933 = FACE_BOUND ( 'NONE', #11644, .T. ) ;
#14934 =( REPRESENTATION_RELATIONSHIP ('NONE','NONE', #11191, #3059 ) REPRESENTATION_RELATIONSHIP_WITH_TRANSFORMATION ( #8387 )SHAPE_REPRESENTATION_RELATIONSHIP( ) );
#14935 = AXIS2_PLACEMENT_3D ( 'NONE', #3766, #3688, #8643 ) ;
#14936 = CARTESIAN_POINT ( 'NONE',  ( -0.06647456835015956578, 227.6089819833846093, 5.110108522575333545 ) ) ;
#14937 = PLANE ( 'NONE',  #13380 ) ;
#14938 = CARTESIAN_POINT ( 'NONE',  ( -1.530808498934191571E-16, 2.500000000000000000, -3.199999997815050623 ) ) ;
#14939 = CARTESIAN_POINT ( 'NONE',  ( -4.946672411965113980E-16, 184.5999999999999943, 9.500000000000001776 ) ) ;
#14940 = CARTESIAN_POINT ( 'NONE',  ( 5.649053410273137565, -2.675685104943120507, 18.61517780375842790 ) ) ;
#14941 = CIRCLE ( 'NONE', #11135, 2.583009025355586186 ) ;
#14943 = EDGE_LOOP ( 'NONE', ( #1215, #2888 ) ) ;
#14942 = CARTESIAN_POINT ( 'NONE',  ( 1.461580736456472795, 188.5499999989075093, 5.538419263543527649 ) ) ;
#14944 = CARTESIAN_POINT ( 'NONE',  ( -6.000000000000000888, 0.000000000000000000, 53.67766952966368876 ) ) ;
#14945 = AXIS2_PLACEMENT_3D ( 'NONE', #7724, #12281, #12574 ) ;
#14946 = EDGE_CURVE ( 'NONE', #7931, #3171, #5214, .T. ) ;
#14947 = CARTESIAN_POINT ( 'NONE',  ( -5.131373506000878493, 7.062729720843910819, 24.49999999999999289 ) ) ;
#14948 = EDGE_CURVE ( 'NONE', #13466, #8455, #48, .T. ) ;
#14949 = CARTESIAN_POINT ( 'NONE',  ( 0.000000000000000000, 186.5669965222008386, 9.317226423031119253 ) ) ;
#14950 = DIRECTION ( 'NONE',  ( 0.000000000000000000, 0.000000000000000000, 1.000000000000000000 ) ) ;
#14951 = CARTESIAN_POINT ( 'NONE',  ( 4.592425496802573972E-16, -2.500000000000000000, 0.2999999999999999334 ) ) ;
#14952 = CARTESIAN_POINT ( 'NONE',  ( 2.252723718013021958, 189.7744973743064918, 9.355516826583022194 ) ) ;
#14953 = CARTESIAN_POINT ( 'NONE',  ( 0.08014973387278834238, -0.3999999999999941380, -2.550381935564455027 ) ) ;
#14954 = B_SPLINE_CURVE_WITH_KNOTS ( 'NONE', 3,
 ( #9655, #14496, #1674, #7805, #405, #7573, #10275, #7649, #6627, #13922, #14976, #12498, #331, #1596, #634, #12728, #8937, #485 ),
 .UNSPECIFIED., .F., .F.,
 ( 4, 2, 2, 2, 2, 2, 2, 2, 4 ),
 ( 0.000000000000000000, 0.0003914898357794939715, 0.0007829796715589879431, 0.001174469507338482023, 0.001565959343117975886, 0.001957449178897469749, 0.002348939014676962745, 0.002740428850456455741, 0.003131918686235948303 ),
 .UNSPECIFIED. ) ;
#14955 = CARTESIAN_POINT ( 'NONE',  ( 3.419318284370305161, -4.932111238568102962, 5.999920023562623328 ) ) ;
#14957 = CARTESIAN_POINT ( 'NONE',  ( -3.312341048453446568, 5.004306261885469453, 30.02601979877761451 ) ) ;
#14956 = CIRCLE ( 'NONE', #14436, 5.000000000000000000 ) ;
#14958 = DIRECTION ( 'NONE',  ( 0.9510565162951499785, 0.3090169943749582204, 0.000000000000000000 ) ) ;
#14959 = CARTESIAN_POINT ( 'NONE',  ( -6.000000000000000000, 0.000000000000000000, 36.00000000000000711 ) ) ;
#14960 = CIRCLE ( 'NONE', #2770, 3.000000000000000000 ) ;
#14961 = ORIENTED_EDGE ( 'NONE', *, *, #7655, .T. ) ;
#14962 = CARTESIAN_POINT ( 'NONE',  ( -1.461580736456473018, 186.3499999989075206, 5.538419263543527649 ) ) ;
#14963 =( BOUNDED_CURVE ( )  B_SPLINE_CURVE ( 2, ( #10061, #14909, #4163, #2737, #15146, #3049, #1844, #5131, #3918 ),
 .UNSPECIFIED., .F., .F. ) 
 B_SPLINE_CURVE_WITH_KNOTS ( ( 3, 2, 2, 2, 3 ),
 ( 0.5000000000000000000, 0.5178571428571429047, 0.5357142857142856984, 0.5535714285714286031, 0.5714285714285713969 ),
 .UNSPECIFIED. ) 
 CURVE ( )  GEOMETRIC_REPRESENTATION_ITEM ( )  RATIONAL_B_SPLINE_CURVE ( ( 1.000000000000000000, 0.9238795325112867385, 1.000000000000000000, 0.9238795325112867385, 1.000000000000000000, 0.9238795325112867385, 1.000000000000000000, 0.9238795325112867385, 1.000000000000000000 ) ) 
 REPRESENTATION_ITEM ( '' )  );
#14964 = ORIENTED_EDGE ( 'NONE', *, *, #15367, .F. ) ;
#14965 = CARTESIAN_POINT ( 'NONE',  ( 0.000000000000000000, 0.000000000000000000, 2.000000000000001776 ) ) ;
#14966 = ORIENTED_EDGE ( 'NONE', *, *, #474, .T. ) ;
#14967 = DIRECTION ( 'NONE',  ( 0.000000000000000000, -0.000000000000000000, 1.000000000000000000 ) ) ;
#14968 = ORIENTED_EDGE ( 'NONE', *, *, #10709, .T. ) ;
#14969 = CARTESIAN_POINT ( 'NONE',  ( -2.066987299999999639, 0.000000000000000000, -1.949999998907525178 ) ) ;
#14970 = CARTESIAN_POINT ( 'NONE',  ( -3.883588957979220879, 4.898466244118957036, 4.026227171247318104 ) ) ;
#14971 = DIRECTION ( 'NONE',  ( 0.000000000000000000, 0.000000000000000000, 1.000000000000000000 ) ) ;
#14972 = CARTESIAN_POINT ( 'NONE',  ( -5.131373506000823426, 7.062729720843950787, 17.99999999999998934 ) ) ;
#14973 = CARTESIAN_POINT ( 'NONE',  ( 2.500000000000000444, 1.035533905932737975, 1.450000002184950176 ) ) ;
#14974 =( BOUNDED_SURFACE ( )  B_SPLINE_SURFACE ( 1, 2, ( 
 ( #10641, #5639, #3239, #777, #12859, #9295, #11904, #5720, #3164, #928, #1013, #9452, #1886, #4363, #13099, #11592, #5875, #8262, #15503, #4601, #2044, #11678, #1964, #7942, #8022, #4441, #4518, #14134, #6917, #8184, #11751, #13021, #15261, #5566, #10722, #2120, #6992, #9223, #4682, #15580, #11821, #5795, #14286, #3393, #2198, #9533, #14370, #8426, #9850, #11035, #12148, #11987, #12300, #1397, #11112, #6273, #133, #217, #55, #15658, #5076, #1322, #2281, #13263, #4922, #12068, #9928, #7230, #7455, #3788, #8859, #3558, #2598, #3474, #8344, #8588, #13182, #2526, #4998, #3635, #7150, #1168, #10957, #1092, #4843, #5955, #10799, #4759, #9616, #13341, #9699, #3712, #8664, #14455, #9777, #14623, #2362, #6036, #10882, #14537, #6198 ),
 ( #8511, #2444, #1247, #7308, #12223, #6122, #14700, #13423, #7382, #13495, #8738, #7850, #15092, #6587, #11423, #8900, #2761, #3941, #14779, #5153, #11269, #7689, #1560, #369, #15017, #5236, #10162, #1478, #7532, #12694, #8979, #1635, #3865, #11498, #1791, #2918, #12459, #13645, #4109, #12539, #13883, #13570, #8816, #5393, #523, #6513, #12378, #6667, #601, #5472, #2680, #10240, #6356, #11346, #11192, #291, #12615, #10008, #7613, #444, #6437, #14854, #10082, #2996, #4186, #14932, #4024, #13735, #2843, #5317, #13808, #7769, #1711, #9058, #10471, #8246, #8003, #2025, #3071, #6822, #995, #2179, #7922, #4267, #4425, #759, #10547, #10627, #9132, #11734, #5702, #6744, #673, #7051, #3151, #15325, #3378, #11807, #11657, #9355, #13080 ),
 ( #9281, #14268, #9436, #837, #11885, #12846, #9203, #10315, #13964, #6975, #5780, #15168, #14118, #15404, #1949, #5624, #3223, #911, #14196, #5548, #8087, #6902, #12926, #12764, #15490, #4501, #4586, #1870, #3302, #8165, #10396, #13003, #11577, #15245, #2104, #4345, #14042, #10705, #39, #2262, #7440, #10783, #8411, #3540, #3457, #13246, #2344, #3695, #7292, #4905, #13163, #14437, #1303, #13480, #4983, #9834, #14519, #2423, #15641, #12051, #8572, #13401, #7212, #2511, #6018, #5936, #15562, #1230, #7365, #4743, #9680, #1150, #10941, #9593, #10859, #1075, #15726, #6180, #3618, #11969, #4824, #13322, #8495, #12129, #2584, #6099, #9762, #12284, #11018, #14604, #12207, #14348, #118, #14683, #3773, #8650, #5858, #4664, #9516, #8324, #7133 ),
 ( #12443, #6337, #1459, #8721, #2744, #6258, #2976, #11096, #7673, #1543, #9910, #12594, #11251, #5375, #506, #12520, #10222, #9989, #273, #1383, #194, #13791, #1694, #15073, #6418, #1619, #8801, #4090, #13630, #5136, #3848, #3924, #11173, #14838, #7595, #8885, #4006, #5057, #9039, #4167, #8960, #13864, #13717, #13554, #7827, #14999, #14764, #352, #2824, #5217, #2663, #10067, #7516, #6570, #14916, #6495, #12362, #11330, #427, #5298, #10146, #2900, #7749, #11405, #10604, #10375, #4409, #5452, #9186, #3358, #4565, #10299, #6648, #6803, #3132, #12907, #12981, #11480, #14098, #8065, #9114, #3054, #9415, #5527, #1929, #5761, #14176, #14026, #11715, #15463, #7985, #1851, #7905, #583, #11558, #6725, #15225, #4328, #3206, #12677, #15151 ) ),
 .UNSPECIFIED., .F., .F., .F. ) 
 B_SPLINE_SURFACE_WITH_KNOTS ( ( 2, 1, 1, 2 ),
 ( 3, 2, 2, 2, 2, 2, 2, 2, 2, 2, 2, 2, 2, 2, 2, 2, 2, 2, 2, 2, 2, 2, 2, 2, 2, 2, 2, 2, 2, 2, 2, 2, 2, 2, 2, 2, 2, 2, 2, 2, 2, 2, 2, 2, 2, 2, 2, 2, 2, 2, 3 ),
 ( -0.1000000000000000056, 0.000000000000000000, 1.000000000000000000, 1.100000000000000089 ),
 ( 0.000000000000000000, 0.01785714285714285615, 0.03571428571428571230, 0.05357142857142856845, 0.07142857142857142461, 0.08928571428571428770, 0.1071428571428571369, 0.1250000000000000000, 0.1428571428571428492, 0.1607142857142857262, 0.1785714285714285754, 0.1964285714285714246, 0.2142857142857142738, 0.2321428571428571508, 0.2500000000000000000, 0.2678571428571428492, 0.2857142857142856984, 0.3035714285714285476, 0.3214285714285714524, 0.3392857142857143016, 0.3571428571428571508, 0.3750000000000000000, 0.3928571428571428492, 0.4107142857142856984, 0.4285714285714285476, 0.4464285714285714524, 0.4642857142857143016, 0.4821428571428571508, 0.5000000000000000000, 0.5178571428571429047, 0.5357142857142856984, 0.5535714285714286031, 0.5714285714285713969, 0.5892857142857143016, 0.6071428571428570953, 0.6250000000000000000, 0.6428571428571429047, 0.6607142857142856984, 0.6785714285714286031, 0.6964285714285713969, 0.7142857142857143016, 0.7321428571428570953, 0.7500000000000000000, 0.7678571428571429047, 0.7857142857142856984, 0.8035714285714286031, 0.8214285714285713969, 0.8392857142857143016, 0.8571428571428570953, 0.8750000000000000000, 0.8928571428571429047 ),
 .UNSPECIFIED. ) 
 GEOMETRIC_REPRESENTATION_ITEM ( )  RATIONAL_B_SPLINE_SURFACE ( (
 ( 1.000000000000000000, 0.9238795325112867385, 1.000000000000000000, 0.9238795325112867385, 1.000000000000000000, 0.9238795325112867385, 1.000000000000000000, 0.9238795325112867385, 1.000000000000000000, 0.9238795325112867385, 1.000000000000000000, 0.9238795325112867385, 1.000000000000000000, 0.9238795325112867385, 1.000000000000000000, 0.9238795325112867385, 1.000000000000000000, 0.9238795325112867385, 1.000000000000000000, 0.9238795325112867385, 1.000000000000000000, 0.9238795325112867385, 1.000000000000000000, 0.9238795325112867385, 1.000000000000000000, 0.9238795325112867385, 1.000000000000000000, 0.9238795325112867385, 1.000000000000000000, 0.9238795325112867385, 1.000000000000000000, 0.9238795325112867385, 1.000000000000000000, 0.9238795325112867385, 1.000000000000000000, 0.9238795325112867385, 1.000000000000000000, 0.9238795325112867385, 1.000000000000000000, 0.9238795325112867385, 1.000000000000000000, 0.9238795325112867385, 1.000000000000000000, 0.9238795325112867385, 1.000000000000000000, 0.9238795325112867385, 1.000000000000000000, 0.9238795325112867385, 1.000000000000000000, 0.9238795325112867385, 1.000000000000000000, 0.9238795325112867385, 1.000000000000000000, 0.9238795325112867385, 1.000000000000000000, 0.9238795325112867385, 1.000000000000000000, 0.9238795325112867385, 1.000000000000000000, 0.9238795325112867385, 1.000000000000000000, 0.9238795325112867385, 1.000000000000000000, 0.9238795325112867385, 1.000000000000000000, 0.9238795325112867385, 1.000000000000000000, 0.9238795325112867385, 1.000000000000000000, 0.9238795325112867385, 1.000000000000000000, 0.9238795325112867385, 1.000000000000000000, 0.9238795325112867385, 1.000000000000000000, 0.9238795325112867385, 1.000000000000000000, 0.9238795325112867385, 1.000000000000000000, 0.9238795325112867385, 1.000000000000000000, 0.9238795325112867385, 1.000000000000000000, 0.9238795325112867385, 1.000000000000000000, 0.9238795325112867385, 1.000000000000000000, 0.9238795325112867385, 1.000000000000000000, 0.9238795325112867385, 1.000000000000000000, 0.9238795325112867385, 1.000000000000000000, 0.9238795325112867385, 1.000000000000000000, 0.9238795325112867385, 1.000000000000000000, 0.9238795325112867385, 1.000000000000000000, 0.9238795325112867385, 1.000000000000000000),
 ( 1.000000000000000000, 0.9238795325112867385, 1.000000000000000000, 0.9238795325112867385, 1.000000000000000000, 0.9238795325112867385, 1.000000000000000000, 0.9238795325112867385, 1.000000000000000000, 0.9238795325112867385, 1.000000000000000000, 0.9238795325112867385, 1.000000000000000000, 0.9238795325112867385, 1.000000000000000000, 0.9238795325112867385, 1.000000000000000000, 0.9238795325112867385, 1.000000000000000000, 0.9238795325112867385, 1.000000000000000000, 0.9238795325112867385, 1.000000000000000000, 0.9238795325112867385, 1.000000000000000000, 0.9238795325112867385, 1.000000000000000000, 0.9238795325112867385, 1.000000000000000000, 0.9238795325112867385, 1.000000000000000000, 0.9238795325112867385, 1.000000000000000000, 0.9238795325112867385, 1.000000000000000000, 0.9238795325112867385, 1.000000000000000000, 0.9238795325112867385, 1.000000000000000000, 0.9238795325112867385, 1.000000000000000000, 0.9238795325112867385, 1.000000000000000000, 0.9238795325112867385, 1.000000000000000000, 0.9238795325112867385, 1.000000000000000000, 0.9238795325112867385, 1.000000000000000000, 0.9238795325112867385, 1.000000000000000000, 0.9238795325112867385, 1.000000000000000000, 0.9238795325112867385, 1.000000000000000000, 0.9238795325112867385, 1.000000000000000000, 0.9238795325112867385, 1.000000000000000000, 0.9238795325112867385, 1.000000000000000000, 0.9238795325112867385, 1.000000000000000000, 0.9238795325112867385, 1.000000000000000000, 0.9238795325112867385, 1.000000000000000000, 0.9238795325112867385, 1.000000000000000000, 0.9238795325112867385, 1.000000000000000000, 0.9238795325112867385, 1.000000000000000000, 0.9238795325112867385, 1.000000000000000000, 0.9238795325112867385, 1.000000000000000000, 0.9238795325112867385, 1.000000000000000000, 0.9238795325112867385, 1.000000000000000000, 0.9238795325112867385, 1.000000000000000000, 0.9238795325112867385, 1.000000000000000000, 0.9238795325112867385, 1.000000000000000000, 0.9238795325112867385, 1.000000000000000000, 0.9238795325112867385, 1.000000000000000000, 0.9238795325112867385, 1.000000000000000000, 0.9238795325112867385, 1.000000000000000000, 0.9238795325112867385, 1.000000000000000000, 0.9238795325112867385, 1.000000000000000000, 0.9238795325112867385, 1.000000000000000000),
 ( 1.000000000000000000, 0.9238795325112867385, 1.000000000000000000, 0.9238795325112867385, 1.000000000000000000, 0.9238795325112867385, 1.000000000000000000, 0.9238795325112867385, 1.000000000000000000, 0.9238795325112867385, 1.000000000000000000, 0.9238795325112867385, 1.000000000000000000, 0.9238795325112867385, 1.000000000000000000, 0.9238795325112867385, 1.000000000000000000, 0.9238795325112867385, 1.000000000000000000, 0.9238795325112867385, 1.000000000000000000, 0.9238795325112867385, 1.000000000000000000, 0.9238795325112867385, 1.000000000000000000, 0.9238795325112867385, 1.000000000000000000, 0.9238795325112867385, 1.000000000000000000, 0.9238795325112867385, 1.000000000000000000, 0.9238795325112867385, 1.000000000000000000, 0.9238795325112867385, 1.000000000000000000, 0.9238795325112867385, 1.000000000000000000, 0.9238795325112867385, 1.000000000000000000, 0.9238795325112867385, 1.000000000000000000, 0.9238795325112867385, 1.000000000000000000, 0.9238795325112867385, 1.000000000000000000, 0.9238795325112867385, 1.000000000000000000, 0.9238795325112867385, 1.000000000000000000, 0.9238795325112867385, 1.000000000000000000, 0.9238795325112867385, 1.000000000000000000, 0.9238795325112867385, 1.000000000000000000, 0.9238795325112867385, 1.000000000000000000, 0.9238795325112867385, 1.000000000000000000, 0.9238795325112867385, 1.000000000000000000, 0.9238795325112867385, 1.000000000000000000, 0.9238795325112867385, 1.000000000000000000, 0.9238795325112867385, 1.000000000000000000, 0.9238795325112867385, 1.000000000000000000, 0.9238795325112867385, 1.000000000000000000, 0.9238795325112867385, 1.000000000000000000, 0.9238795325112867385, 1.000000000000000000, 0.9238795325112867385, 1.000000000000000000, 0.9238795325112867385, 1.000000000000000000, 0.9238795325112867385, 1.000000000000000000, 0.9238795325112867385, 1.000000000000000000, 0.9238795325112867385, 1.000000000000000000, 0.9238795325112867385, 1.000000000000000000, 0.9238795325112867385, 1.000000000000000000, 0.9238795325112867385, 1.000000000000000000, 0.9238795325112867385, 1.000000000000000000, 0.9238795325112867385, 1.000000000000000000, 0.9238795325112867385, 1.000000000000000000, 0.9238795325112867385, 1.000000000000000000, 0.9238795325112867385, 1.000000000000000000),
 ( 1.000000000000000000, 0.9238795325112867385, 1.000000000000000000, 0.9238795325112867385, 1.000000000000000000, 0.9238795325112867385, 1.000000000000000000, 0.9238795325112867385, 1.000000000000000000, 0.9238795325112867385, 1.000000000000000000, 0.9238795325112867385, 1.000000000000000000, 0.9238795325112867385, 1.000000000000000000, 0.9238795325112867385, 1.000000000000000000, 0.9238795325112867385, 1.000000000000000000, 0.9238795325112867385, 1.000000000000000000, 0.9238795325112867385, 1.000000000000000000, 0.9238795325112867385, 1.000000000000000000, 0.9238795325112867385, 1.000000000000000000, 0.9238795325112867385, 1.000000000000000000, 0.9238795325112867385, 1.000000000000000000, 0.9238795325112867385, 1.000000000000000000, 0.9238795325112867385, 1.000000000000000000, 0.9238795325112867385, 1.000000000000000000, 0.9238795325112867385, 1.000000000000000000, 0.9238795325112867385, 1.000000000000000000, 0.9238795325112867385, 1.000000000000000000, 0.9238795325112867385, 1.000000000000000000, 0.9238795325112867385, 1.000000000000000000, 0.9238795325112867385, 1.000000000000000000, 0.9238795325112867385, 1.000000000000000000, 0.9238795325112867385, 1.000000000000000000, 0.9238795325112867385, 1.000000000000000000, 0.9238795325112867385, 1.000000000000000000, 0.9238795325112867385, 1.000000000000000000, 0.9238795325112867385, 1.000000000000000000, 0.9238795325112867385, 1.000000000000000000, 0.9238795325112867385, 1.000000000000000000, 0.9238795325112867385, 1.000000000000000000, 0.9238795325112867385, 1.000000000000000000, 0.9238795325112867385, 1.000000000000000000, 0.9238795325112867385, 1.000000000000000000, 0.9238795325112867385, 1.000000000000000000, 0.9238795325112867385, 1.000000000000000000, 0.9238795325112867385, 1.000000000000000000, 0.9238795325112867385, 1.000000000000000000, 0.9238795325112867385, 1.000000000000000000, 0.9238795325112867385, 1.000000000000000000, 0.9238795325112867385, 1.000000000000000000, 0.9238795325112867385, 1.000000000000000000, 0.9238795325112867385, 1.000000000000000000, 0.9238795325112867385, 1.000000000000000000, 0.9238795325112867385, 1.000000000000000000, 0.9238795325112867385, 1.000000000000000000, 0.9238795325112867385, 1.000000000000000000, 0.9238795325112867385, 1.000000000000000000) ) ) 
 REPRESENTATION_ITEM ( '' )  SURFACE ( )  );
#14975 = CARTESIAN_POINT ( 'NONE',  ( 7.347881242120658060E-16, 6.000000000000000888, 4.000000000000004441 ) ) ;
#14976 = CARTESIAN_POINT ( 'NONE',  ( -3.735642931251015320, -4.696778275484483345, 10.52591947216897239 ) ) ;
#14977 = CARTESIAN_POINT ( 'NONE',  ( -1.035533905932739751, 186.9500000000000171, 9.500000000000000000 ) ) ;
#14978 = CARTESIAN_POINT ( 'NONE',  ( 0.8561741729129463963, -2.066987299999999195, 0.9000000010924746885 ) ) ;
#14979 = CARTESIAN_POINT ( 'NONE',  ( 6.155973317223302210, -1.081218830693633670, 10.99691356133952169 ) ) ;
#14980 = CARTESIAN_POINT ( 'NONE',  ( -2.500000000000003109, 186.6499999978150299, 5.964466094067263136 ) ) ;
#14981 = ORIENTED_EDGE ( 'NONE', *, *, #14770, .F. ) ;
#14982 = COLOUR_RGB ( '', 0.72549020, 0.75294118, 0.79215686) ;
#14983 = EDGE_LOOP ( 'NONE', ( #6242, #13598, #15039, #3193 ) ) ;
#14984 = VERTEX_POINT ( 'NONE', #12061 ) ;
#14985 = CARTESIAN_POINT ( 'NONE',  ( 7.000000000000006217, 0.000000000000000000, 0.000000000000000000 ) ) ;
#14986 = CARTESIAN_POINT ( 'NONE',  ( 4.435347140101010943, 4.403429997944537710, 4.867658743658316745 ) ) ;
#14987 = B_SPLINE_CURVE_WITH_KNOTS ( 'NONE', 3,
 ( #15368, #5665, #4464, #9395, #9318, #14233, #8208, #13045, #5822, #10664, #15524, #9725, #13211, #2551, #4786, #9952, #13287, #10907 ),
 .UNSPECIFIED., .F., .F.,
 ( 4, 2, 2, 2, 2, 2, 2, 2, 4 ),
 ( 0.003131918686235956543, 0.003523310662250248981, 0.003914702638264540985, 0.004306094614278833423, 0.004697486590293125860, 0.005088878566307418298, 0.005480270542321710736, 0.005871662518336003174, 0.006263054494350295612 ),
 .UNSPECIFIED. ) ;
#14988 = ORIENTED_EDGE ( 'NONE', *, *, #2105, .F. ) ;
#14989 = CARTESIAN_POINT ( 'NONE',  ( -6.142844459177212890, -1.156093792145330479, 17.38439807107078749 ) ) ;
#14990 = CARTESIAN_POINT ( 'NONE',  ( 0.9999502950802301449, -5.916088184763877322, 31.13108149190011176 ) ) ;
#14991 = CARTESIAN_POINT ( 'NONE',  ( -5.317509234263968487, 2.779225709350972906, 5.130616955321390726 ) ) ;
#14992 = CARTESIAN_POINT ( 'NONE',  ( 2.500000000000000444, -1.035533905932737309, -1.949999999999999956 ) ) ;
#14993 = CARTESIAN_POINT ( 'NONE',  ( 2.500000000000000444, 186.3499999978150754, 5.964466094067262247 ) ) ;
#14994 = EDGE_CURVE ( 'NONE', #11999, #14255, #3870, .T. ) ;
#14995 = LINE ( 'NONE', #650, #13351 ) ;
#14996 = VECTOR ( 'NONE', #2092, 1000.000000000000000 ) ;
#14997 = CARTESIAN_POINT ( 'NONE',  ( 5.747343991580207145, 1.727858744772199584, 18.99992002356260556 ) ) ;
#14998 = CARTESIAN_POINT ( 'NONE',  ( 0.000000000000000000, 64.00000000000000000, 0.000000000000000000 ) ) ;
#14999 = CARTESIAN_POINT ( 'NONE',  ( 1.035533905932738197, 187.0199999975965568, 9.500000000000003553 ) ) ;
#15000 = CARTESIAN_POINT ( 'NONE',  ( 1.326034168411047265, 228.1562120337857777, 9.877435289762864556 ) ) ;
#15001 = ADVANCED_FACE ( 'NONE', ( #10872 ), #9525, .F. ) ;
#15002 = CARTESIAN_POINT ( 'NONE',  ( -1.747606509155581689, 226.5054486174500994, 5.018058692477180394 ) ) ;
#15003 = EDGE_LOOP ( 'NONE', ( #10717, #658 ) ) ;
#15004 = CARTESIAN_POINT ( 'NONE',  ( -0.8150890167390612007, 189.0566948412773343, 10.07644837850013531 ) ) ;
#15005 = AXIS2_PLACEMENT_3D ( 'NONE', #1302, #12283, #10782 ) ;
#15006 = ORIENTED_EDGE ( 'NONE', *, *, #3583, .F. ) ;
#15007 = CARTESIAN_POINT ( 'NONE',  ( -6.172639027853111138, 0.9816353142772042961, 17.73774718278285434 ) ) ;
#15008 = CARTESIAN_POINT ( 'NONE',  ( -6.155867707731091265, 1.081837891426014941, 23.99563030319847812 ) ) ;
#15009 = CARTESIAN_POINT ( 'NONE',  ( -0.9735954530125274786, 6.173909381473990265, 5.262817935852436513 ) ) ;
#15010 = CARTESIAN_POINT ( 'NONE',  ( 0.9737778612007512713, 5.920671847850482727, 24.23736375884649874 ) ) ;
#15011 = CARTESIAN_POINT ( 'NONE',  ( 2.774089264892111384, 227.6570220514033167, 8.409174098727280722 ) ) ;
#15012 = CARTESIAN_POINT ( 'NONE',  ( -2.841519077896096590, -5.566940434250041925, 31.26379616840806719 ) ) ;
#15013 = CARTESIAN_POINT ( 'NONE',  ( -0.8561741729129455081, 2.066987299999999639, -1.099999998907525089 ) ) ;
#15014 = CARTESIAN_POINT ( 'NONE',  ( 3.922396193919041263, 4.541970110199453181, 4.126193172852894442 ) ) ;
#15015 = PRESENTATION_STYLE_ASSIGNMENT (( #6742 ) ) ;
#15016 = DIRECTION ( 'NONE',  ( 0.000000000000000000, 1.000000000000000000, 0.000000000000000000 ) ) ;
#15017 = CARTESIAN_POINT ( 'NONE',  ( -2.500000000000000444, 185.2000000000000171, 7.000000000000000000 ) ) ;
#15018 = CARTESIAN_POINT ( 'NONE',  ( 1.581415667291661276, 227.8641612386227848, 5.847080766174051369 ) ) ;
#15019 = FACE_OUTER_BOUND ( 'NONE', #6848, .T. ) ;
#15020 = CARTESIAN_POINT ( 'NONE',  ( 4.290381260516221928, 4.545736887716255836, 12.11517780375842790 ) ) ;
#15021 = CARTESIAN_POINT ( 'NONE',  ( 0.8561741729129465073, -2.066987299999999195, 1.500000001092474555 ) ) ;
#15022 = CARTESIAN_POINT ( 'NONE',  ( -1.461580736456473906, 188.7499999989075263, 8.461580736456474128 ) ) ;
#15023 = CARTESIAN_POINT ( 'NONE',  ( 5.558508435838292350, -2.857531096718732844, 18.13237410716305220 ) ) ;
#15025 = ORIENTED_EDGE ( 'NONE', *, *, #13123, .F. ) ;
#15024 = CARTESIAN_POINT ( 'NONE',  ( 0.8561741729129455081, 188.5999999989074922, 4.933012699999999029 ) ) ;
#15026 = FACE_BOUND ( 'NONE', #10635, .T. ) ;
#15027 = CARTESIAN_POINT ( 'NONE',  ( -2.500000000000000444, 186.6999999978150697, 7.000000000000000000 ) ) ;
#15028 = CARTESIAN_POINT ( 'NONE',  ( -5.408775798201205021, 2.598833957129572436, 4.386022610569177083 ) ) ;
#15029 = FILL_AREA_STYLE ('',( #15183 ) ) ;
#15030 = CARTESIAN_POINT ( 'NONE',  ( 2.392413146961774206, 188.9999999991792947, 7.742749230693430462 ) ) ;
#15031 = CARTESIAN_POINT ( 'NONE',  ( 0.03893478199943582047, -0.3999999999999923617, -2.531455901217069204 ) ) ;
#15032 = CARTESIAN_POINT ( 'NONE',  ( 5.487097279078464673, -2.429065649168742347, 10.70047945897284336 ) ) ;
#15033 = FACE_OUTER_BOUND ( 'NONE', #12311, .T. ) ;
#15034 = DIRECTION ( 'NONE',  ( 0.000000000000000000, -1.000000000000000000, 0.000000000000000000 ) ) ;
#15035 = DIRECTION ( 'NONE',  ( -0.3090169943749584425, 0.9510565162951498674, 0.000000000000000000 ) ) ;
#15036 = VERTEX_POINT ( 'NONE', #3704 ) ;
#15037 = CARTESIAN_POINT ( 'NONE',  ( -1.016439536705160407E-17, 186.2499999989074979, 4.933012699999999029 ) ) ;
#15038 = EDGE_CURVE ( 'NONE', #4950, #13528, #10791, .T. ) ;
#15039 = ORIENTED_EDGE ( 'NONE', *, *, #13485, .T. ) ;
#15040 = CARTESIAN_POINT ( 'NONE',  ( -5.940390500375820615, 6.474944468551430354, 24.49999999999999289 ) ) ;
#15041 = ORIENTED_EDGE ( 'NONE', *, *, #2004, .T. ) ;
#15042 = DIRECTION ( 'NONE',  ( -0.3090169943749584425, 0.9510565162951498674, 0.000000000000000000 ) ) ;
#15043 = LINE ( 'NONE', #5731, #9385 ) ;
#15044 = VERTEX_POINT ( 'NONE', #13333 ) ;
#15045 = CARTESIAN_POINT ( 'NONE',  ( -5.486741141153769874, -2.429871531109777383, 30.20111757752059134 ) ) ;
#15046 = CARTESIAN_POINT ( 'NONE',  ( -4.154121946520915820, 4.670585111242934850, 4.201121615766615136 ) ) ;
#15047 = FACE_OUTER_BOUND ( 'NONE', #4332, .T. ) ;
#15048 = CARTESIAN_POINT ( 'NONE',  ( -2.500000000000000444, 1.035533905932737753, -2.350000000000000533 ) ) ;
#15049 = DIRECTION ( 'NONE',  ( 0.000000000000000000, 0.000000000000000000, 1.000000000000000000 ) ) ;
#15050 = EDGE_CURVE ( 'NONE', #9099, #660, #15574, .T. ) ;
#15051 = CARTESIAN_POINT ( 'NONE',  ( -2.692693252389710690, 5.362085866495045927, 17.73617396794403689 ) ) ;
#15052 = CARTESIAN_POINT ( 'NONE',  ( -1.035533905932737753, 2.500000000000000444, -0.7499999978150503344 ) ) ;
#15053 = CARTESIAN_POINT ( 'NONE',  ( 2.066987300000000083, -0.8561741729129449530, -1.399999998907525134 ) ) ;
#15054 =( BOUNDED_CURVE ( )  B_SPLINE_CURVE ( 2, ( #8534, #1190, #7253, #13363, #12173, #9641, #3581, #11138, #6144 ),
 .UNSPECIFIED., .F., .F. ) 
 B_SPLINE_CURVE_WITH_KNOTS ( ( 3, 2, 2, 2, 3 ),
 ( 0.5714285714285713969, 0.5892857142857143016, 0.6071428571428570953, 0.6250000000000000000, 0.6428571428571429047 ),
 .UNSPECIFIED. ) 
 CURVE ( )  GEOMETRIC_REPRESENTATION_ITEM ( )  RATIONAL_B_SPLINE_CURVE ( ( 1.000000000000000000, 0.9238795325112867385, 1.000000000000000000, 0.9238795325112867385, 1.000000000000000000, 0.9238795325112867385, 1.000000000000000000, 0.9238795325112867385, 1.000000000000000000 ) ) 
 REPRESENTATION_ITEM ( '' )  );
#15055 = CARTESIAN_POINT ( 'NONE',  ( -0.3932117513507903395, 228.2473332724799207, 10.14534249745510586 ) ) ;
#15056 = ADVANCED_FACE ( 'NONE', ( #10715 ), #1005, .T. ) ;
#15057 = ORIENTED_EDGE ( 'NONE', *, *, #3458, .T. ) ;
#15058 = AXIS2_PLACEMENT_3D ( 'NONE', #8699, #13842, #6312 ) ;
#15059 = VERTEX_POINT ( 'NONE', #12216 ) ;
#15060 = ORIENTED_EDGE ( 'NONE', *, *, #8486, .F. ) ;
#15061 = CARTESIAN_POINT ( 'NONE',  ( 4.416397290909928941, -4.422724436066409304, 11.76379616840804232 ) ) ;
#15062 = CARTESIAN_POINT ( 'NONE',  ( 6.081590040723058976, 1.446205118473082862, 4.126326713640078303 ) ) ;
#15063 = VERTEX_POINT ( 'NONE', #8658 ) ;
#15064 = CARTESIAN_POINT ( 'NONE',  ( -3.000000000000000000, 0.000000000000000000, 5.000000000000004441 ) ) ;
#15065 = CARTESIAN_POINT ( 'NONE',  ( 0.2622538972265521795, -6.245673238944470462, 18.97385994369199480 ) ) ;
#15066 = CARTESIAN_POINT ( 'NONE',  ( -5.620879908643986234, 2.102487719021839840, 5.973778239432934178 ) ) ;
#15067 = CARTESIAN_POINT ( 'NONE',  ( 0.8738239080081156018, 6.188820299975580141, 18.50355795710150986 ) ) ;
#15068 = CARTESIAN_POINT ( 'NONE',  ( -2.500000000000000444, 185.1499999978150584, 8.035533905932737753 ) ) ;
#15069 = CIRCLE ( 'NONE', #9994, 2.000000000000000000 ) ;
#15070 = CARTESIAN_POINT ( 'NONE',  ( 1.767766952966368654, 1.767766952966369098, 2.206999999978150662 ) ) ;
#15071 = CARTESIAN_POINT ( 'NONE',  ( -3.779082820360787132, 4.979770177899181860, 19.00004906876531763 ) ) ;
#15072 = DIRECTION ( 'NONE',  ( 0.000000000000000000, 0.000000000000000000, 1.000000000000000000 ) ) ;
#15073 = CARTESIAN_POINT ( 'NONE',  ( -2.500000000000000444, 185.9199999975965625, 5.964466094067261359 ) ) ;
#15074 = CARTESIAN_POINT ( 'NONE',  ( 1.865071889996124055, 228.0459258470066857, 9.553136980667057188 ) ) ;
#15075 = CARTESIAN_POINT ( 'NONE',  ( -2.623350778723538834, 226.8212935938476278, 5.948734516926445615 ) ) ;
#15076 = EDGE_LOOP ( 'NONE', ( #882, #2145, #11222, #12625 ) ) ;
#15077 = CARTESIAN_POINT ( 'NONE',  ( -0.6887091348229088528, -2.420707839511175408, -2.499422994081509586 ) ) ;
#15078 = EDGE_CURVE ( 'NONE', #6002, #6522, #8821, .T. ) ;
#15079 = ORIENTED_EDGE ( 'NONE', *, *, #3402, .T. ) ;
#15080 = CARTESIAN_POINT ( 'NONE',  ( -2.841519077896279999, 5.566940434249946890, 17.73620383159192926 ) ) ;
#15081 = CARTESIAN_POINT ( 'NONE',  ( -5.984595133899138553, 1.806709459528792916, 23.50004921015706216 ) ) ;
#15082 = PRODUCT_DEFINITION ( 'UNKNOWN', '', #687, #4348 ) ;
#15083 = CARTESIAN_POINT ( 'NONE',  ( -0.8002720181890968787, 6.199262377003405433, 4.386062624655573394 ) ) ;
#15084 = CARTESIAN_POINT ( 'NONE',  ( 5.649200442566169933, 2.675373855294122638, 12.11560192892920718 ) ) ;
#15085 = CARTESIAN_POINT ( 'NONE',  ( 1.359424073589828197, 228.1503905913944834, 9.860327814513095035 ) ) ;
#15086 = CARTESIAN_POINT ( 'NONE',  ( -3.459447313391792012, -5.206669755181024151, 31.97400098023329917 ) ) ;
#15087 = CARTESIAN_POINT ( 'NONE',  ( -4.344762547369755090, -4.493114738039176714, 18.50308643866044278 ) ) ;
#15088 = CARTESIAN_POINT ( 'NONE',  ( 2.066987299999999639, 2.531329380823229670E-16, -1.349999998907525534 ) ) ;
#15089 = CARTESIAN_POINT ( 'NONE',  ( -3.634089073485383903, -4.776071126502727360, 31.99992002356261978 ) ) ;
#15090 = TOROIDAL_SURFACE ( 'NONE', #5443, 2.483389555546409166, 0.1000000000000000056 ) ;
#15091 = CARTESIAN_POINT ( 'NONE',  ( -7.490007020835705909, -2.433650805992367161, 5.000000000000004441 ) ) ;
#15092 = CARTESIAN_POINT ( 'NONE',  ( -4.946672411965113980E-16, 184.5999999999999943, 9.500000000000001776 ) ) ;
#15093 = CARTESIAN_POINT ( 'NONE',  ( 0.1304739971030711432, 227.6100227634930775, 5.113114354890055502 ) ) ;
#15094 = FACE_BOUND ( 'NONE', #9268, .T. ) ;
#15095 = B_SPLINE_CURVE_WITH_KNOTS ( 'NONE', 3,
 ( #8243, #10781, #3538, #9831, #3846, #8493, #8799, #3922, #37, #271, #12360, #2742, #9678, #9987, #6256, #14836, #1381, #12049 ),
 .UNSPECIFIED., .F., .F.,
 ( 4, 2, 2, 2, 2, 2, 2, 2, 4 ),
 ( 0.000000000000000000, 0.0003914904498596255512, 0.0007829808997192511024, 0.001174471349578876545, 0.001565961799438502205, 0.001957452249298127864, 0.002348942699157753090, 0.002740433149017378750, 0.003131923598877004410 ),
 .UNSPECIFIED. ) ;
#15096 = CARTESIAN_POINT ( 'NONE',  ( -2.500000000000000000, 0.000000000000000000, -2.999999997815050889 ) ) ;
#15097 = CARTESIAN_POINT ( 'NONE',  ( 0.07162589071487505954, 189.0001276426230561, 4.501026264287848910 ) ) ;
#15098 = CARTESIAN_POINT ( 'NONE',  ( -2.500000000000000444, 185.2499999999999716, 8.035533905932737753 ) ) ;
#15099 = CARTESIAN_POINT ( 'NONE',  ( -5.487348639458818234, -2.428538342494575453, 18.80022217383878669 ) ) ;
#15100 = EDGE_CURVE ( 'NONE', #9290, #3041, #11651, .T. ) ;
#15102 = ORIENTED_EDGE ( 'NONE', *, *, #7218, .F. ) ;
#15101 = CARTESIAN_POINT ( 'NONE',  ( -0.8561741729129455081, 187.0999999989075206, 4.933012699999999029 ) ) ;
#15103 = CARTESIAN_POINT ( 'NONE',  ( -4.286401442266628337, -4.198423832313095794, 17.99999999999998934 ) ) ;
#15104 = CARTESIAN_POINT ( 'NONE',  ( 5.903230462362985875, -1.077253041748709173, 17.38557478428062097 ) ) ;
#15105 = CARTESIAN_POINT ( 'NONE',  ( 0.000000000000000000, 222.7460571280668091, 12.08513476933103625 ) ) ;
#15106 = FILL_AREA_STYLE ('',( #4122 ) ) ;
#15107 = CARTESIAN_POINT ( 'NONE',  ( 2.461882965037902160, 189.3814125599426745, 5.297573457840181632 ) ) ;
#15108 = FACE_OUTER_BOUND ( 'NONE', #6941, .T. ) ;
#15109 = CARTESIAN_POINT ( 'NONE',  ( -5.866984344570842502, -1.259800266528583013, 5.799318062581741984 ) ) ;
#15110 = CARTESIAN_POINT ( 'NONE',  ( 2.977271291746630411, 189.8591517725882625, 7.726790542730640254 ) ) ;
#15111 = CARTESIAN_POINT ( 'NONE',  ( 5.770331821586412779, -2.404225004693576029, 5.873800552473965375 ) ) ;
#15112 = CARTESIAN_POINT ( 'NONE',  ( 0.09128442572436945568, 0.4000000000000010214, 2.551849451885215725 ) ) ;
#15113 = DIRECTION ( 'NONE',  ( 0.9510565162951500895, 0.3090169943749582204, 0.000000000000000000 ) ) ;
#15114 = EDGE_LOOP ( 'NONE', ( #8847, #2863 ) ) ;
#15115 = CARTESIAN_POINT ( 'NONE',  ( 2.066987300000000527, 185.8499999989074922, 7.000000000000000000 ) ) ;
#15116 = ORIENTED_EDGE ( 'NONE', *, *, #11106, .T. ) ;
#15117 = CARTESIAN_POINT ( 'NONE',  ( -5.903057025253874102, -1.078199533779696573, 23.88438267301394191 ) ) ;
#15118 = ADVANCED_FACE ( 'NONE', ( #5068 ), #4178, .F. ) ;
#15119 = ORIENTED_EDGE ( 'NONE', *, *, #6021, .F. ) ;
#15120 = FACE_OUTER_BOUND ( 'NONE', #10185, .T. ) ;
#15121 = CARTESIAN_POINT ( 'NONE',  ( -2.500000000000000444, 185.9500000000000455, 5.964466094067261359 ) ) ;
#15122 = CARTESIAN_POINT ( 'NONE',  ( -3.420311045507748116, -4.931422832349356966, 6.000079611744768115 ) ) ;
#15123 = CARTESIAN_POINT ( 'NONE',  ( -4.435347140101074004, 4.403429997944470209, 4.869393092765016640 ) ) ;
#15124 = CARTESIAN_POINT ( 'NONE',  ( -4.435347140101009167, -4.403429997944534158, 5.130606907234994019 ) ) ;
#15125 = CARTESIAN_POINT ( 'NONE',  ( -1.767766952966368432, -1.767766952966369320, -1.400000000000000133 ) ) ;
#15126 = EDGE_CURVE ( 'NONE', #10812, #10806, #2338, .T. ) ;
#15127 = CARTESIAN_POINT ( 'NONE',  ( -6.172639027853119131, -0.9816353142771574447, 5.262252817217141221 ) ) ;
#15128 = CLOSED_SHELL ( 'NONE', ( #9031, #10865, #8786, #3797, #1329, #3694, #2180, #9812, #2629, #7753, #4952, #4245, #5805, #8136, #11046, #12358, #14591, #3087, #5564, #12210, #12765, #3174, #2433, #683, #12553, #6691, #4152 ) ) ;
#15129 = DIRECTION ( 'NONE',  ( 0.000000000000000000, 0.000000000000000000, 1.000000000000000000 ) ) ;
#15130 = CIRCLE ( 'NONE', #10057, 1.499999999999999556 ) ;
#15131 = FACE_OUTER_BOUND ( 'NONE', #8695, .T. ) ;
#15132 = CARTESIAN_POINT ( 'NONE',  ( -2.066987299999999195, -0.8561741729129466183, 0.7000000010924749549 ) ) ;
#15133 = CARTESIAN_POINT ( 'NONE',  ( -0.4907341119409533992, 228.2426455014340263, 10.13156071145469639 ) ) ;
#15134 = ORIENTED_EDGE ( 'NONE', *, *, #15250, .T. ) ;
#15135 = ORIENTED_EDGE ( 'NONE', *, *, #7132, .F. ) ;
#15136 = VERTEX_POINT ( 'NONE', #282 ) ;
#15137 = CARTESIAN_POINT ( 'NONE',  ( -6.105861027178945299, -1.337741388557017963, 10.70045537531157542 ) ) ;
#15138 = DIRECTION ( 'NONE',  ( 1.000000000000000000, 0.000000000000000000, 0.000000000000000000 ) ) ;
#15139 = AXIS2_PLACEMENT_3D ( 'NONE', #1956, #2034, #12773 ) ;
#15140 = ORIENTED_EDGE ( 'NONE', *, *, #11106, .F. ) ;
#15141 = FILL_AREA_STYLE_COLOUR ( '', #15223 ) ;
#15142 = CARTESIAN_POINT ( 'NONE',  ( 2.500000000000000444, -1.035533905932737309, -1.049999997815050490 ) ) ;
#15143 =( REPRESENTATION_RELATIONSHIP ('NONE','NONE', #11191, #3660 ) REPRESENTATION_RELATIONSHIP_WITH_TRANSFORMATION ( #2401 )SHAPE_REPRESENTATION_RELATIONSHIP( ) );
#15144 = EDGE_CURVE ( 'NONE', #6851, #2492, #6843, .T. ) ;
#15145 = CARTESIAN_POINT ( 'NONE',  ( -5.317509234263969375, 2.779225709350973350, 5.000000000000004441 ) ) ;
#15146 = CARTESIAN_POINT ( 'NONE',  ( -6.844026213814746740E-16, 187.6999999978150697, 9.500000000000001776 ) ) ;
#15147 = CARTESIAN_POINT ( 'NONE',  ( 1.035533905932737753, 188.8499999978150470, 4.500000000000000888 ) ) ;
#15148 = CARTESIAN_POINT ( 'NONE',  ( 0.8499999999999896527, 0.000000000000000000, 0.000000000000000000 ) ) ;
#15149 = EDGE_CURVE ( 'NONE', #898, #6574, #7458, .T. ) ;
#15150 = CARTESIAN_POINT ( 'NONE',  ( 5.867109477881248480, 1.259218163100889631, 18.79888242247938734 ) ) ;
#15151 = CARTESIAN_POINT ( 'NONE',  ( -1.998997755520148800E-16, 189.7699999975965568, 4.500000000000000000 ) ) ;
#15152 = CARTESIAN_POINT ( 'NONE',  ( -0.8817132232236292166, 228.8448810635624682, 8.679455557192847337 ) ) ;
#15153 = CARTESIAN_POINT ( 'NONE',  ( -2.668764612700158079, 227.7307401636093687, 8.626063590916809076 ) ) ;
#15154 = VERTEX_POINT ( 'NONE', #7760 ) ;
#15155 = CARTESIAN_POINT ( 'NONE',  ( -1.113756821657925000, 2.256897984573015048, -2.499694356362072156 ) ) ;
#15156 = VERTEX_POINT ( 'NONE', #5146 ) ;
#15157 = CARTESIAN_POINT ( 'NONE',  ( 2.930600586413043107, -5.520563544161711356, 5.503086438660451662 ) ) ;
#15158 = CARTESIAN_POINT ( 'NONE',  ( -6.000000000000000000, 0.000000000000000000, 0.000000000000000000 ) ) ;
#15159 = DIRECTION ( 'NONE',  ( 0.9510565162951499785, 0.3090169943749582204, 0.000000000000000000 ) ) ;
#15160 = CARTESIAN_POINT ( 'NONE',  ( 0.000000000000000000, 22.00000000000000000, 0.000000000000000000 ) ) ;
#15161 = CARTESIAN_POINT ( 'NONE',  ( -7.799024015210601846, -1.482594289697409140, 24.49999999999999289 ) ) ;
#15162 = AXIS2_PLACEMENT_3D ( 'NONE', #6825, #11661, #6904 ) ;
#15163 = CARTESIAN_POINT ( 'NONE',  ( -3.061616997868391523E-16, 189.0000000000000000, 7.000000000000000000 ) ) ;
#15164 = CARTESIAN_POINT ( 'NONE',  ( 3.779681992289775749, -4.979315417303914693, 17.00004921015705506 ) ) ;
#15165 = CARTESIAN_POINT ( 'NONE',  ( 1.035533905932737531, 2.500000000000000444, 0.6500000000000000222 ) ) ;
#15166 = CARTESIAN_POINT ( 'NONE',  ( -1.265664690411614835E-16, 2.066987299999999639, -2.749999998907525001 ) ) ;
#15167 = CARTESIAN_POINT ( 'NONE',  ( -4.435347140101024266, -4.403429997944519947, 31.00000000000000000 ) ) ;
#15168 = CARTESIAN_POINT ( 'NONE',  ( -1.035533905932739529, 185.2499999978150811, 9.500000000000003553 ) ) ;
#15169 = CARTESIAN_POINT ( 'NONE',  ( -0.6092285535620440839, 227.6401390286306992, 5.200091846327095979 ) ) ;
#15170 = FACE_BOUND ( 'NONE', #13046, .T. ) ;
#15171 = CARTESIAN_POINT ( 'NONE',  ( 0.7988860301924620710, 6.199427171881305654, 23.88455580536198397 ) ) ;
#15172 = CARTESIAN_POINT ( 'NONE',  ( 0.8561741729129465073, -2.066987299999999195, -1.699999998907525400 ) ) ;
#15173 = CARTESIAN_POINT ( 'NONE',  ( -7.420008617947670970E-16, 188.5999999999999943, 9.500000000000001776 ) ) ;
#15174 = CARTESIAN_POINT ( 'NONE',  ( 1.353717517954364224E-13, -6.250000000000000888, 17.99999999999998934 ) ) ;
#15176 = VERTEX_POINT ( 'NONE', #14773 ) ;
#15175 = CARTESIAN_POINT ( 'NONE',  ( 1.461580736456472351, 188.3499999989074922, 8.461580736456474128 ) ) ;
#15177 = EDGE_CURVE ( 'NONE', #1121, #12191, #9546, .T. ) ;
#15178 = CYLINDRICAL_SURFACE ( 'NONE', #4322, 1.500000000000000000 ) ;
#15179 = B_SPLINE_CURVE_WITH_KNOTS ( 'NONE', 3,
 ( #8043, #14075, #3496, #15520, #8204, #10432, #2300, #8368, #9472, #3257, #4459, #5818, #13040, #4702, #4386, #10508, #11925, #13117 ),
 .UNSPECIFIED., .F., .F.,
 ( 4, 2, 2, 2, 2, 2, 2, 2, 4 ),
 ( 0.003131486019301986824, 0.003522824630466693530, 0.003914163241631400669, 0.004305501852796107809, 0.004696840463960814081, 0.005088179075125520354, 0.005479517686290226626, 0.005870856297454932898, 0.006262194908619639171 ),
 .UNSPECIFIED. ) ;
#15180 = CARTESIAN_POINT ( 'NONE',  ( 5.317509234264033324, -2.779225709350853002, 17.86763921416088152 ) ) ;
#15181 = VECTOR ( 'NONE', #304, 1000.000000000000000 ) ;
#15182 = CARTESIAN_POINT ( 'NONE',  ( -5.842945980534631545, 1.369128644669023176, 23.62621569129737509 ) ) ;
#15183 = FILL_AREA_STYLE_COLOUR ( '', #4563 ) ;
#15184 = EDGE_CURVE ( 'NONE', #7351, #3463, #8810, .T. ) ;
#15185 = CARTESIAN_POINT ( 'NONE',  ( 2.687945937111228645, 189.8130902236854070, 8.690539078995184852 ) ) ;
#15186 = CARTESIAN_POINT ( 'NONE',  ( 2.500000000000000444, 187.9499999978150697, 5.964466094067262247 ) ) ;
#15187 = CYLINDRICAL_SURFACE ( 'NONE', #11359, 12.50000000000000533 ) ;
#15188 = CARTESIAN_POINT ( 'NONE',  ( 1.974798917232459150, 228.1755836975312945, 6.746486589875083872 ) ) ;
#15189 = CARTESIAN_POINT ( 'NONE',  ( 6.155973317223325303, -1.081218830693501998, 23.99691356133952169 ) ) ;
#15190 = CARTESIAN_POINT ( 'NONE',  ( -6.081464507797648800, 1.446657058464131840, 4.126199447526042619 ) ) ;
#15191 = CARTESIAN_POINT ( 'NONE',  ( -3.107688324358644838, -5.133887830459872958, 30.12621569129737154 ) ) ;
#15192 = ORIENTED_EDGE ( 'NONE', *, *, #10955, .T. ) ;
#15193 = CARTESIAN_POINT ( 'NONE',  ( 1.461580736456472573, 186.5499999989075093, 8.461580736456474128 ) ) ;
#15194 = CIRCLE ( 'NONE', #3004, 5.000000000000000000 ) ;
#15195 = B_SPLINE_CURVE_WITH_KNOTS ( 'NONE', 1,
 ( #12057, #8416 ),
 .UNSPECIFIED., .F., .F.,
 ( 2, 2 ),
 ( 0.000000000000000000, 1.000000000000000000 ),
 .UNSPECIFIED. ) ;
#15196 = CARTESIAN_POINT ( 'NONE',  ( 3.010624175977964612, 5.190832888732229478, 30.20111757752060200 ) ) ;
#15197 = CIRCLE ( 'NONE', #13659, 12.49999999999999822 ) ;
#15198 = ORIENTED_EDGE ( 'NONE', *, *, #5079, .T. ) ;
#15199 = CARTESIAN_POINT ( 'NONE',  ( -5.131373506000715068, 7.062729720844030723, 5.000000000000004441 ) ) ;
#15200 = CARTESIAN_POINT ( 'NONE',  ( -5.317509234263919637, -2.779225709351067053, 30.86938304467861016 ) ) ;
#15201 = CARTESIAN_POINT ( 'NONE',  ( 1.354942165200771727E-13, 6.000000000000000888, 16.99999999999998579 ) ) ;
#15202 = AXIS2_PLACEMENT_3D ( 'NONE', #9027, #7972, #4397 ) ;
#15203 = LINE ( 'NONE', #9238, #10233 ) ;
#15204 = CARTESIAN_POINT ( 'NONE',  ( -2.500000000000000000, -1.035533905932739307, -0.6500000000000000222 ) ) ;
#15205 = CARTESIAN_POINT ( 'NONE',  ( -1.767766952966369098, 1.767766952966369098, 2.400000000000000355 ) ) ;
#15206 = CARTESIAN_POINT ( 'NONE',  ( 5.999999999999999112, 215.7452399395091618, 13.29567785264566027 ) ) ;
#15207 = CARTESIAN_POINT ( 'NONE',  ( -1.767766952966369098, 1.767766952966369098, -0.6999999978150501789 ) ) ;
#15208 = CARTESIAN_POINT ( 'NONE',  ( 1.461580736456472573, 1.461580736456472795, -2.049999998907525267 ) ) ;
#15209 = CARTESIAN_POINT ( 'NONE',  ( 0.000000000000000000, 186.4999999978150527, 4.500000000000000000 ) ) ;
#15210 = EDGE_LOOP ( 'NONE', ( #5, #6148 ) ) ;
#15211 = EDGE_LOOP ( 'NONE', ( #2114, #1740, #9007, #3044 ) ) ;
#15212 = AXIS2_PLACEMENT_3D ( 'NONE', #14845, #4174, #3211 ) ;
#15213 = EDGE_LOOP ( 'NONE', ( #3967, #2148, #9171, #6243 ) ) ;
#15214 = CARTESIAN_POINT ( 'NONE',  ( -6.172552660730974416, -0.9821660343539097004, 11.23620383159194880 ) ) ;
#15215 = FACE_BOUND ( 'NONE', #44, .T. ) ;
#15216 = ORIENTED_EDGE ( 'NONE', *, *, #7543, .F. ) ;
#15217 = CARTESIAN_POINT ( 'NONE',  ( -2.500000000000000444, 1.035533905932737753, 1.750000002184949777 ) ) ;
#15218 = CARTESIAN_POINT ( 'NONE',  ( -5.935543223013843850, -0.8771126767607685393, 31.13239388001635177 ) ) ;
#15219 = CARTESIAN_POINT ( 'NONE',  ( 2.897581130414634077E-17, 22.00000000000000000, 9.750000000000003553 ) ) ;
#15220 = CARTESIAN_POINT ( 'NONE',  ( 2.066987300000000083, 185.2499999989074979, 7.000000000000000000 ) ) ;
#15221 = CARTESIAN_POINT ( 'NONE',  ( 2.500000000000000444, -1.035533905932737309, 2.056999999978150306 ) ) ;
#15222 = CARTESIAN_POINT ( 'NONE',  ( -4.291255145204149635, 4.544933371694606095, 18.61396179408071561 ) ) ;
#15223 = COLOUR_RGB ( '', 0.08235294, 0.09019608, 0.10196078) ;
#15224 = CARTESIAN_POINT ( 'NONE',  ( 3.796994071234844259E-16, -2.066987299999999639, 1.450000001092474733 ) ) ;
#15225 = CARTESIAN_POINT ( 'NONE',  ( 2.500000000000000000, 189.5699999975965397, 7.000000000000000000 ) ) ;
#15226 = CARTESIAN_POINT ( 'NONE',  ( -0.8219475227482178070, 228.8541360017199224, 8.706184346459185264 ) ) ;
#15227 = CARTESIAN_POINT ( 'NONE',  ( -0.9647310034392982958, 228.2043607281333379, 10.01900208526334168 ) ) ;
#15228 = ORIENTED_EDGE ( 'NONE', *, *, #1713, .F. ) ;
#15229 = ADVANCED_FACE ( 'NONE', ( #2093 ), #2017, .T. ) ;
#15230 = CARTESIAN_POINT ( 'NONE',  ( 2.503681785030714479, -0.03945699161127848992, -2.499748181185309281 ) ) ;
#15231 = ORIENTED_EDGE ( 'NONE', *, *, #355, .T. ) ;
#15232 = ADVANCED_FACE ( 'NONE', ( #14186, #901, #4258, #14033, #5770, #750 ), #1862, .F. ) ;
#15233 = CARTESIAN_POINT ( 'NONE',  ( -0.1306394121198675706, 6.250000000000001776, 10.49999999999998579 ) ) ;
#15234 = B_SPLINE_CURVE_WITH_KNOTS ( 'NONE', 3,
 ( #3840, #12353, #1449, #7430, #6327, #3995, #4079, #8713, #6485, #9825, #8640, #2655, #6408, #13546, #5127, #1685, #13472, #9979 ),
 .UNSPECIFIED., .F., .F.,
 ( 4, 2, 2, 2, 2, 2, 2, 2, 4 ),
 ( 0.003131490185286086615, 0.003522829482338686678, 0.003914168779391286740, 0.004305508076443887236, 0.004696847373496487732, 0.005088186670549088228, 0.005479525967601688724, 0.005870865264654288353, 0.006262204561706888849 ),
 .UNSPECIFIED. ) ;
#15235 = DIRECTION ( 'NONE',  ( 0.8660254037844385966, -0.4999999999999998890, 0.000000000000000000 ) ) ;
#15236 = CARTESIAN_POINT ( 'NONE',  ( 6.155912734541151288, 1.081577393120788821, 23.99610786875030044 ) ) ;
#15237 = ORIENTED_EDGE ( 'NONE', *, *, #5612, .T. ) ;
#15238 = CYLINDRICAL_SURFACE ( 'NONE', #8435, 1.000000000000000222 ) ;
#15239 = FACE_BOUND ( 'NONE', #12643, .T. ) ;
#15240 = CARTESIAN_POINT ( 'NONE',  ( 3.159612573729182028, -5.393342049074657751, 17.19973484982323697 ) ) ;
#15241 = CARTESIAN_POINT ( 'NONE',  ( -2.500000000000000000, 0.000000000000000000, 0.09999999999999982514 ) ) ;
#15242 = CARTESIAN_POINT ( 'NONE',  ( -3.736532060717939085, -4.696070028786012429, 31.97377823943293151 ) ) ;
#15243 = SHAPE_REPRESENTATION_RELATIONSHIP ( 'NONE' , 'NONE' ,  #9569, #4039 ) ;
#15244 = LINE ( 'NONE', #4344, #7012 ) ;
#15245 = CARTESIAN_POINT ( 'NONE',  ( 2.500000000000000444, 186.3499999978150754, 5.964466094067262247 ) ) ;
#15247 = CARTESIAN_POINT ( 'NONE',  ( 1.747590535343585438, 228.0744605602133674, 9.637048244069795544 ) ) ;
#15246 = STYLED_ITEM ( 'NONE', ( #12924 ), #10501 ) ;
#15248 = CARTESIAN_POINT ( 'NONE',  ( 1.353717517954364224E-13, -6.250000000000000888, 17.99999999999998934 ) ) ;
#15249 = CARTESIAN_POINT ( 'NONE',  ( 0.6156133477427582212, 6.220296490279936030, 25.29872387345520579 ) ) ;
#15250 = EDGE_CURVE ( 'NONE', #14086, #5348, #15481, .T. ) ;
#15251 = CARTESIAN_POINT ( 'NONE',  ( -1.265664690411614835E-16, 2.066987299999999639, -2.149999998907525800 ) ) ;
#15252 = CARTESIAN_POINT ( 'NONE',  ( -1.767766952966369320, 185.9000000000000057, 5.232233047033630235 ) ) ;
#15253 = CARTESIAN_POINT ( 'NONE',  ( 2.996920846510414460, -5.485395142346829900, 25.11441947245483419 ) ) ;
#15255 = ORIENTED_EDGE ( 'NONE', *, *, #9844, .F. ) ;
#15254 = CARTESIAN_POINT ( 'NONE',  ( 0.000000000000000000, 0.000000000000000000, 0.000000000000000000 ) ) ;
#15256 = CARTESIAN_POINT ( 'NONE',  ( -3.061616997868391523E-16, 189.0000000000000000, 9.500000000000000000 ) ) ;
#15257 = CARTESIAN_POINT ( 'NONE',  ( 0.09128442572411965550, -0.3999999999999975797, 2.551849451881568420 ) ) ;
#15258 = CARTESIAN_POINT ( 'NONE',  ( -2.389652190990207536, 189.9828712853605168, 5.408448231032084941 ) ) ;
#15259 = SURFACE_STYLE_USAGE ( .BOTH. , #6451 ) ;
#15260 = CARTESIAN_POINT ( 'NONE',  ( 0.7947751900520840795, 189.0000000008628831, 4.622669032342844098 ) ) ;
#15261 = CARTESIAN_POINT ( 'NONE',  ( 2.500000000000000444, 185.5300000002184788, 7.000000000000000000 ) ) ;
#15262 = CARTESIAN_POINT ( 'NONE',  ( -0.2619456584321807613, 5.995505046955615924, 30.02607193928647433 ) ) ;
#15263 = B_SPLINE_CURVE_WITH_KNOTS ( 'NONE', 3,
 ( #13471, #2573, #5048, #6325, #11008, #7429, #8871, #10055, #3839, #2654, #10135, #8638, #263, #7507, #5202, #13702, #14986, #14904 ),
 .UNSPECIFIED., .F., .F.,
 ( 4, 2, 2, 2, 2, 2, 2, 2, 4 ),
 ( 0.003131486019301986824, 0.003522824630466693096, 0.003914163241631399802, 0.004305501852796106074, 0.004696840463960812347, 0.005088179075125518619, 0.005479517686290224891, 0.005870856297454931164, 0.006262194908619637436 ),
 .UNSPECIFIED. ) ;
#15264 = CARTESIAN_POINT ( 'NONE',  ( 1.986724198295925836, 228.2179917342068052, 6.868963418589798309 ) ) ;
#15265 = CARTESIAN_POINT ( 'NONE',  ( 5.984377695197236946, -1.807429553002246614, 6.000049068765331839 ) ) ;
#15266 = CARTESIAN_POINT ( 'NONE',  ( 2.500000000000000444, 184.0000000000000000, 7.000000000000000000 ) ) ;
#15267 = CARTESIAN_POINT ( 'NONE',  ( 2.500000000000000444, -1.035533905932737309, 1.350000002184949865 ) ) ;
#15268 = VERTEX_POINT ( 'NONE', #10462 ) ;
#15270 = CARTESIAN_POINT ( 'NONE',  ( 2.066987300000000083, 185.7999999989075093, 7.856174172912946396 ) ) ;
#15269 = PRODUCT_DEFINITION_SHAPE ( 'NONE', 'NONE',  #3310 ) ;
#15271 = CARTESIAN_POINT ( 'NONE',  ( 1.734723475976807094E-15, 0.000000000000000000, 15.50000000000000000 ) ) ;
#15272 = B_SPLINE_CURVE_WITH_KNOTS ( 'NONE', 3,
 ( #1268, #14482, #14395, #10981, #2303, #6062, #6223, #2385, #9640, #3656, #3500, #12011, #9557, #4785, #9797, #12090, #4705, #8371 ),
 .UNSPECIFIED., .F., .F.,
 ( 4, 2, 2, 2, 2, 2, 2, 2, 4 ),
 ( 0.000000000000000000, 0.0003914357524127468893, 0.0007828715048254937785, 0.001174307257238240559, 0.001565743009650987557, 0.001957178762063732820, 0.002348614514476478517, 0.002740050266889223780, 0.003131486019301969476 ),
 .UNSPECIFIED. ) ;
#15273 = ORIENTED_EDGE ( 'NONE', *, *, #6110, .T. ) ;
#15274 = EDGE_CURVE ( 'NONE', #1681, #13364, #11404, .T. ) ;
#15275 = CARTESIAN_POINT ( 'NONE',  ( -2.500000000000000888, 188.2999999978150356, 7.000000000000000000 ) ) ;
#15276 = CARTESIAN_POINT ( 'NONE',  ( -2.897581130414634077E-17, 22.00000000000000000, -9.750000000000003553 ) ) ;
#15277 = CARTESIAN_POINT ( 'NONE',  ( -5.935543223013844738, -0.8771126767607686503, 30.86763921416089573 ) ) ;
#15278 = CARTESIAN_POINT ( 'NONE',  ( 1.035533905932737531, 2.500000000000000444, -0.04999999781505021224 ) ) ;
#15279 = LINE ( 'NONE', #8039, #3739 ) ;
#15280 = CARTESIAN_POINT ( 'NONE',  ( 1.461580736456473462, 184.3499999989074922, 5.538419263543526760 ) ) ;
#15281 = CARTESIAN_POINT ( 'NONE',  ( -2.997753866155722591, -5.484939622623898003, 5.615601928929210729 ) ) ;
#15282 = CARTESIAN_POINT ( 'NONE',  ( 2.500000000000000444, -1.035533905932737309, -0.2499999978150503066 ) ) ;
#15283 = CARTESIAN_POINT ( 'NONE',  ( 3.922288969639810663, -4.542045818322500317, 10.62621569129736976 ) ) ;
#15284 = CARTESIAN_POINT ( 'NONE',  ( 0.000000000000000000, 186.5669965222008386, 9.317226423031119253 ) ) ;
#15285 = DIRECTION ( 'NONE',  ( 1.000000000000000000, 0.000000000000000000, 0.000000000000000000 ) ) ;
#15286 = CARTESIAN_POINT ( 'NONE',  ( -5.409007216690611131, -2.598315788643874136, 17.38557478428061742 ) ) ;
#15287 = CARTESIAN_POINT ( 'NONE',  ( 5.131373506000546314, 7.062729720844130199, 11.49999999999998224 ) ) ;
#15288 = ORIENTED_EDGE ( 'NONE', *, *, #1274, .F. ) ;
#15289 = B_SPLINE_CURVE_WITH_KNOTS ( 'NONE', 3,
 ( #12612, #1708, #520, #13962, #5470, #5391, #10238, #15242, #15089, #4184, #9055, #13880, #4582, #15486, #13244, #4498, #8083, #12923 ),
 .UNSPECIFIED., .F., .F.,
 ( 4, 2, 2, 2, 2, 2, 2, 2, 4 ),
 ( 0.003131918686235972155, 0.003523310662250262858, 0.003914702638264553995, 0.004306094614278844698, 0.004697486590293134534, 0.005088878566307424370, 0.005480270542321714206, 0.005871662518336004041, 0.006263054494350293010 ),
 .UNSPECIFIED. ) ;
#15290 = ORIENTED_EDGE ( 'NONE', *, *, #11808, .F. ) ;
#15291 = ORIENTED_EDGE ( 'NONE', *, *, #8070, .F. ) ;
#15292 = VECTOR ( 'NONE', #11493, 1000.000000000000000 ) ;
#15293 = CARTESIAN_POINT ( 'NONE',  ( 3.780072143464223711, -4.979057943639742412, 12.50008219321555103 ) ) ;
#15294 = DIRECTION ( 'NONE',  ( 0.000000000000000000, 0.000000000000000000, 1.000000000000000000 ) ) ;
#15295 = ORIENTED_EDGE ( 'NONE', *, *, #7586, .F. ) ;
#15296 =( LENGTH_UNIT ( ) NAMED_UNIT ( * ) SI_UNIT ( .MILLI., .METRE. ) );
#15297 = PRODUCT_DEFINITION_SHAPE ( 'NONE', 'NONE',  #10321 ) ;
#15298 = CARTESIAN_POINT ( 'NONE',  ( -2.500000000000000000, 0.000000000000000000, -0.5999999978150505342 ) ) ;
#15299 = CARTESIAN_POINT ( 'NONE',  ( 6.106056299406759535, 1.336851112280623921, 18.79887838423337598 ) ) ;
#15300 = DIRECTION ( 'NONE',  ( 0.000000000000000000, 0.000000000000000000, 1.000000000000000000 ) ) ;
#15301 = CARTESIAN_POINT ( 'NONE',  ( -1.456896669277396583E-16, 188.8999999978150584, 4.500000000000000000 ) ) ;
#15302 = CARTESIAN_POINT ( 'NONE',  ( -1.530808498934191571E-16, 2.500000000000000000, 1.506999999978150706 ) ) ;
#15303 = DIRECTION ( 'NONE',  ( 0.000000000000000000, 0.000000000000000000, 1.000000000000000000 ) ) ;
#15304 = CARTESIAN_POINT ( 'NONE',  ( -0.8561741729129458411, -2.066987299999999195, 0.6000000010924746441 ) ) ;
#15305 = AXIS2_PLACEMENT_3D ( 'NONE', #1280, #9886, #12182 ) ;
#15306 = CARTESIAN_POINT ( 'NONE',  ( -5.931734679891446760, -0.9039278060244212432, 4.736173967944048435 ) ) ;
#15307 = CARTESIAN_POINT ( 'NONE',  ( 0.6359992007181909379, 226.3469529472061765, 4.550856198837272437 ) ) ;
#15308 = DIRECTION ( 'NONE',  ( -0.000000000000000000, 1.000000000000000000, -0.000000000000000000 ) ) ;
#15309 = ORIENTED_EDGE ( 'NONE', *, *, #2500, .T. ) ;
#15310 = CARTESIAN_POINT ( 'NONE',  ( -2.290915817347055849, 1.041596279477050135, -2.500307733819811862 ) ) ;
#15311 = ORIENTED_EDGE ( 'NONE', *, *, #11196, .F. ) ;
#15312 = FACE_OUTER_BOUND ( 'NONE', #14735, .T. ) ;
#15313 = ADVANCED_FACE ( 'NONE', ( #7994 ), #5463, .F. ) ;
#15314 = CARTESIAN_POINT ( 'NONE',  ( 2.999999999999999556, -1.732050807568877859, -5.500000000000000000 ) ) ;
#15315 = PRODUCT_DEFINITION ( 'UNKNOWN', '', #6300, #11500 ) ;
#15316 = DIRECTION ( 'NONE',  ( 0.000000000000000000, 0.000000000000000000, -1.000000000000000000 ) ) ;
#15318 = VERTEX_POINT ( 'NONE', #11798 ) ;
#15317 = VECTOR ( 'NONE', #8144, 1000.000000000000114 ) ;
#15319 = CYLINDRICAL_SURFACE ( 'NONE', #9457, 2.500000000000000444 ) ;
#15320 = FACE_BOUND ( 'NONE', #5767, .T. ) ;
#15321 = B_SPLINE_CURVE_WITH_KNOTS ( 'NONE', 3,
 ( #7527, #3936, #12689, #1787, #6661, #1632, #596, #4260, #5388, #6508, #14927, #8812, #4019, #8895, #11341, #438, #10235, #9128 ),
 .UNSPECIFIED., .F., .F.,
 ( 4, 2, 2, 2, 2, 2, 2, 2, 4 ),
 ( 0.000000000000000000, 0.0003914357524127489493, 0.0007828715048254978985, 0.001174307257238246848, 0.001565743009650994713, 0.001957178762063743228, 0.002348614514476490660, 0.002740050266889238959, 0.003131486019301986824 ),
 .UNSPECIFIED. ) ;
#15322 = CARTESIAN_POINT ( 'NONE',  ( -1.530808498934191571E-16, 2.500000000000000000, 0.6999999999999998446 ) ) ;
#15323 = CARTESIAN_POINT ( 'NONE',  ( -4.416678568553779272, -4.422441866694181378, 24.76236973443873168 ) ) ;
#15324 = DIRECTION ( 'NONE',  ( 0.000000000000000000, 0.000000000000000000, -1.000000000000000000 ) ) ;
#15325 = CARTESIAN_POINT ( 'NONE',  ( 2.500000000000000000, 188.7500000000000000, 8.035533905932739529 ) ) ;
#15326 = EDGE_CURVE ( 'NONE', #5344, #11668, #4816, .T. ) ;
#15327 = CARTESIAN_POINT ( 'NONE',  ( -1.974809306405319154, 228.1756194782155944, 6.746589926531873616 ) ) ;
#15328 = FACE_BOUND ( 'NONE', #11960, .T. ) ;
#15329 = EDGE_CURVE ( 'NONE', #13541, #6640, #3368, .T. ) ;
#15330 = CARTESIAN_POINT ( 'NONE',  ( 0.2623718222037388359, 6.245654667075775990, 23.52627829713835439 ) ) ;
#15331 = APPLICATION_CONTEXT ( 'automotive_design' ) ;
#15332 = CARTESIAN_POINT ( 'NONE',  ( -2.066987299999999639, 0.000000000000000000, -2.749999998907525445 ) ) ;
#15333 = CARTESIAN_POINT ( 'NONE',  ( 1.035533905932738197, 187.8500000000000227, 9.500000000000003553 ) ) ;
#15334 = DIRECTION ( 'NONE',  ( -1.000000000000000000, 3.326610055774643275E-18, -1.062480551894329622E-17 ) ) ;
#15336 = ORIENTED_EDGE ( 'NONE', *, *, #10673, .F. ) ;
#15335 = CARTESIAN_POINT ( 'NONE',  ( 5.000000000000000000, 6.123233995736766282E-16, 5.000000000000004441 ) ) ;
#15337 = LINE ( 'NONE', #3083, #6121 ) ;
#15338 = ORIENTED_EDGE ( 'NONE', *, *, #275, .T. ) ;
#15339 = CARTESIAN_POINT ( 'NONE',  ( -9.750000000000003553, 3.401296724241641415E-14, 2.000000000000001776 ) ) ;
#15340 = DIRECTION ( 'NONE',  ( -0.000000000000000000, 1.000000000000000000, -0.000000000000000000 ) ) ;
#15341 = EDGE_CURVE ( 'NONE', #6786, #6278, #7267, .T. ) ;
#15342 = SURFACE_SIDE_STYLE ('',( #8103 ) ) ;
#15343 = CARTESIAN_POINT ( 'NONE',  ( -1.035533905932738197, -2.500000000000000000, -0.4499999978150504010 ) ) ;
#15344 = DIRECTION ( 'NONE',  ( 0.8090169943749421222, 0.5877852522924802425, 0.000000000000000000 ) ) ;
#15345 = LINE ( 'NONE', #13902, #4505 ) ;
#15346 = CARTESIAN_POINT ( 'NONE',  ( 1.581415667291661276, 227.8641612386227848, 5.847080766174051369 ) ) ;
#15347 = FACE_BOUND ( 'NONE', #10386, .T. ) ;
#15348 = CARTESIAN_POINT ( 'NONE',  ( 2.082642335314403343E-14, 6.000000000000000888, 32.00000000000000000 ) ) ;
#15349 = CARTESIAN_POINT ( 'NONE',  ( -2.500000000000000000, 0.000000000000000000, 1.000000002184949777 ) ) ;
#15350 = B_SPLINE_CURVE_WITH_KNOTS ( 'NONE', 3,
 ( #6670, #11503, #604, #13969, #3077, #7925, #7744, #13859, #6489, #13624, #577, #13709, #12671, #4240, #5293, #2817, #6412, #7666 ),
 .UNSPECIFIED., .F., .F.,
 ( 4, 2, 2, 2, 2, 2, 2, 2, 4 ),
 ( 0.003131486019301976849, 0.003522824630466684856, 0.003914163241631392863, 0.004305501852796100870, 0.004696840463960809745, 0.005088179075125516884, 0.005479517686290225759, 0.005870856297454933766, 0.006262194908619641773 ),
 .UNSPECIFIED. ) ;
#15351 = EDGE_CURVE ( 'NONE', #11236, #8072, #5383, .T. ) ;
#15352 = ORIENTED_EDGE ( 'NONE', *, *, #4948, .T. ) ;
#15353 = CARTESIAN_POINT ( 'NONE',  ( 2.066987299999999195, 189.1999999989075434, 7.856174172912946396 ) ) ;
#15354 = CARTESIAN_POINT ( 'NONE',  ( 4.141923667210638094, 4.342011609040473452, 30.38438267301394902 ) ) ;
#15355 = VERTEX_POINT ( 'NONE', #3607 ) ;
#15356 = CARTESIAN_POINT ( 'NONE',  ( -4.286401442266532413, -4.198423832313194382, 4.869350386511452911 ) ) ;
#15357 =( BOUNDED_CURVE ( )  B_SPLINE_CURVE ( 2, ( #9401, #8213, #11777, #5904, #143, #13127, #3800, #14313, #12233, #6282, #7098, #961, #13049, #15452, #11044, #9786, #14237, #4553, #14633, #3874, #5827, #6946, #11935, #1041, #3722, #8600, #7391, #5007, #8674, #7467, #12310, #11122, #9936, #14788, #12969, #2072, #13816, #1487, #12388, #4034, #377, #12703, #10249, #2689, #5162, #13892, #7541, #1799, #9066, #531, #5401, #2851, #12467, #15101, #13743, #1722, #3005, #608, #2928, #11507, #4197, #7777, #10016, #10325, #13655, #11278, #6445, #6365, #5246, #10091, #6596, #10169, #12624, #301, #1569, #7863, #5481, #6674, #15175, #1645, #5325, #8747, #14942, #15024, #7623, #8826, #4117, #453, #11201, #13579, #14864, #3952, #11431, #8909, #7699, #2771, #12548, #6521, #11355, #8989, #10403 ),
 .UNSPECIFIED., .F., .F. ) 
 B_SPLINE_CURVE_WITH_KNOTS ( ( 3, 2, 2, 2, 2, 2, 2, 2, 2, 2, 2, 2, 2, 2, 2, 2, 2, 2, 2, 2, 2, 2, 2, 2, 2, 2, 2, 2, 2, 2, 2, 2, 2, 2, 2, 2, 2, 2, 2, 2, 2, 2, 2, 2, 2, 2, 2, 2, 2, 2, 3 ),
 ( 0.000000000000000000, 0.01785714285714285615, 0.03571428571428571230, 0.05357142857142856845, 0.07142857142857142461, 0.08928571428571428770, 0.1071428571428571369, 0.1250000000000000000, 0.1428571428571428492, 0.1607142857142857262, 0.1785714285714285754, 0.1964285714285714246, 0.2142857142857142738, 0.2321428571428571508, 0.2500000000000000000, 0.2678571428571428492, 0.2857142857142856984, 0.3035714285714285476, 0.3214285714285714524, 0.3392857142857143016, 0.3571428571428571508, 0.3750000000000000000, 0.3928571428571428492, 0.4107142857142856984, 0.4285714285714285476, 0.4464285714285714524, 0.4642857142857143016, 0.4821428571428571508, 0.5000000000000000000, 0.5178571428571429047, 0.5357142857142856984, 0.5535714285714286031, 0.5714285714285713969, 0.5892857142857143016, 0.6071428571428570953, 0.6250000000000000000, 0.6428571428571429047, 0.6607142857142856984, 0.6785714285714286031, 0.6964285714285715079, 0.7142857142857143016, 0.7321428571428570953, 0.7500000000000000000, 0.7678571428571429047, 0.7857142857142856984, 0.8035714285714286031, 0.8214285714285713969, 0.8392857142857143016, 0.8571428571428570953, 0.8750000000000000000, 0.8928571428571429047 ),
 .UNSPECIFIED. ) 
 CURVE ( )  GEOMETRIC_REPRESENTATION_ITEM ( )  RATIONAL_B_SPLINE_CURVE ( ( 1.000000000000000000, 0.9238795325112867385, 1.000000000000000000, 0.9238795325112867385, 1.000000000000000000, 0.9238795325112867385, 1.000000000000000000, 0.9238795325112867385, 1.000000000000000000, 0.9238795325112867385, 1.000000000000000000, 0.9238795325112867385, 1.000000000000000000, 0.9238795325112867385, 1.000000000000000000, 0.9238795325112867385, 1.000000000000000000, 0.9238795325112867385, 1.000000000000000000, 0.9238795325112867385, 1.000000000000000000, 0.9238795325112867385, 1.000000000000000000, 0.9238795325112867385, 1.000000000000000000, 0.9238795325112867385, 1.000000000000000000, 0.9238795325112867385, 1.000000000000000000, 0.9238795325112867385, 1.000000000000000000, 0.9238795325112867385, 1.000000000000000000, 0.9238795325112867385, 1.000000000000000000, 0.9238795325112867385, 1.000000000000000000, 0.9238795325112867385, 1.000000000000000000, 0.9238795325112867385, 1.000000000000000000, 0.9238795325112867385, 1.000000000000000000, 0.9238795325112867385, 1.000000000000000000, 0.9238795325112867385, 1.000000000000000000, 0.9238795325112867385, 1.000000000000000000, 0.9238795325112867385, 1.000000000000000000, 0.9238795325112867385, 1.000000000000000000, 0.9238795325112867385, 1.000000000000000000, 0.9238795325112867385, 1.000000000000000000, 0.9238795325112867385, 1.000000000000000000, 0.9238795325112867385, 1.000000000000000000, 0.9238795325112867385, 1.000000000000000000, 0.9238795325112867385, 1.000000000000000000, 0.9238795325112867385, 1.000000000000000000, 0.9238795325112867385, 1.000000000000000000, 0.9238795325112867385, 1.000000000000000000, 0.9238795325112867385, 1.000000000000000000, 0.9238795325112867385, 1.000000000000000000, 0.9238795325112867385, 1.000000000000000000, 0.9238795325112867385, 1.000000000000000000, 0.9238795325112867385, 1.000000000000000000, 0.9238795325112867385, 1.000000000000000000, 0.9238795325112867385, 1.000000000000000000, 0.9238795325112867385, 1.000000000000000000, 0.9238795325112867385, 1.000000000000000000, 0.9238795325112867385, 1.000000000000000000, 0.9238795325112867385, 1.000000000000000000, 0.9238795325112867385, 1.000000000000000000, 0.9238795325112867385, 1.000000000000000000, 0.9238795325112867385, 1.000000000000000000, 0.9238795325112867385, 1.000000000000000000 ) ) 
 REPRESENTATION_ITEM ( '' )  );
#15358 = DIRECTION ( 'NONE',  ( -0.9510565162951545304, 0.3090169943749447867, 0.000000000000000000 ) ) ;
#15359 = CARTESIAN_POINT ( 'NONE',  ( 5.935543223013868719, 0.8771126767606117758, 17.86935038651144936 ) ) ;
#15360 = CARTESIAN_POINT ( 'NONE',  ( 1.461580736456473462, 185.9499999989075150, 5.538419263543526760 ) ) ;
#15361 = CARTESIAN_POINT ( 'NONE',  ( 5.931793676715125585, -0.9035324301686619153, 24.23760108194402108 ) ) ;
#15362 = CARTESIAN_POINT ( 'NONE',  ( -2.500000000000000444, 1.035533905932737753, -1.449999997815050401 ) ) ;
#15363 = CARTESIAN_POINT ( 'NONE',  ( 2.126728311762493650E-16, 22.00000000000000000, 8.250000000000003553 ) ) ;
#15364 = CARTESIAN_POINT ( 'NONE',  ( 5.999999999999999112, 188.6555110544239824, 3.692234042173051289 ) ) ;
#15365 = DIRECTION ( 'NONE',  ( -0.9510565162951544194, 0.3090169943749447312, 0.000000000000000000 ) ) ;
#15366 = CARTESIAN_POINT ( 'NONE',  ( 4.153663429050758360, 4.670992970568392799, 31.79933148907576523 ) ) ;
#15367 = EDGE_CURVE ( 'NONE', #8616, #7973, #4694, .T. ) ;
#15368 = CARTESIAN_POINT ( 'NONE',  ( 5.935543223013856284, 0.8771126767606806096, 11.49999999999998224 ) ) ;
#15369 = AXIS2_PLACEMENT_3D ( 'NONE', #6629, #5508, #3035 ) ;
#15370 = VERTEX_POINT ( 'NONE', #7282 ) ;
#15371 = VERTEX_POINT ( 'NONE', #6006 ) ;
#15372 = VERTEX_POINT ( 'NONE', #14510 ) ;
#15373 = CARTESIAN_POINT ( 'NONE',  ( -6.020865209844587618, -1.681180471732168780, 10.52599901976669194 ) ) ;
#15374 = CARTESIAN_POINT ( 'NONE',  ( 5.558508435838190209, 2.857531096718933128, 4.867625892836953128 ) ) ;
#15375 = ORIENTED_EDGE ( 'NONE', *, *, #13774, .F. ) ;
#15376 = CARTESIAN_POINT ( 'NONE',  ( 1.035533905932737531, 2.500000000000000444, -0.04999999781505042734 ) ) ;
#15377 = CARTESIAN_POINT ( 'NONE',  ( -5.866984344570836285, -1.259800266528611878, 31.79931806258174376 ) ) ;
#15378 = LINE ( 'NONE', #966, #10512 ) ;
#15379 = CARTESIAN_POINT ( 'NONE',  ( -9.825582188149883933E-17, 188.0999999978150754, 4.500000000000000000 ) ) ;
#15380 = CARTESIAN_POINT ( 'NONE',  ( -1.767766952966368432, -1.767766952966369320, 0.2069999999781506062 ) ) ;
#15381 = DIRECTION ( 'NONE',  ( -0.3090169943749579429, 0.9510565162951502005, 0.000000000000000000 ) ) ;
#15382 = PRODUCT_CONTEXT ( 'NONE', #5877, 'mechanical' ) ;
#15383 = CARTESIAN_POINT ( 'NONE',  ( -2.066987299999999639, 0.000000000000000000, 0.4500000010924747329 ) ) ;
#15384 = EDGE_CURVE ( 'NONE', #1214, #10844, #11009, .T. ) ;
#15385 = CARTESIAN_POINT ( 'NONE',  ( 4.435347140101073116, -4.403429997944470209, 5.000000000000004441 ) ) ;
#15386 = CARTESIAN_POINT ( 'NONE',  ( 2.899241599682305992, 227.5396000034540975, 8.063657412308430139 ) ) ;
#15387 = CARTESIAN_POINT ( 'NONE',  ( -0.3932117513507903395, 228.2473332724799207, 10.14534249745510586 ) ) ;
#15388 = ADVANCED_FACE ( 'NONE', ( #8563 ), #13389, .F. ) ;
#15389 = B_SPLINE_CURVE_WITH_KNOTS ( 'NONE', 3,
 ( #6623, #15123, #2873, #629, #400, #15046, #11224, #14970, #12416, #10346, #5186, #10040, #12571, #13764, #2953, #12723, #2795, #7800 ),
 .UNSPECIFIED., .F., .F.,
 ( 4, 2, 2, 2, 2, 2, 2, 2, 4 ),
 ( 0.003131486019301987257, 0.003522824630466693530, 0.003914163241631399802, 0.004305501852796106074, 0.004696840463960813214, 0.005088179075125520354, 0.005479517686290226626, 0.005870856297454934633, 0.006262194908619640905 ),
 .UNSPECIFIED. ) ;
#15390 = ORIENTED_EDGE ( 'NONE', *, *, #12497, .T. ) ;
#15391 = CARTESIAN_POINT ( 'NONE',  ( -2.500000000000000444, 185.9499999978150697, 8.035533905932737753 ) ) ;
#15392 = CIRCLE ( 'NONE', #4200, 4.000000000000001776 ) ;
#15393 = VERTEX_POINT ( 'NONE', #15553 ) ;
#15394 = CARTESIAN_POINT ( 'NONE',  ( 3.882809187879016299, -4.899079348629983954, 5.974000980233302727 ) ) ;
#15395 = CARTESIAN_POINT ( 'NONE',  ( 4.286401442266496886, -4.198423832313229020, 17.99999999999998934 ) ) ;
#15396 = DIRECTION ( 'NONE',  ( -1.000000000000000000, 0.000000000000000000, 0.000000000000000000 ) ) ;
#15397 = ORIENTED_EDGE ( 'NONE', *, *, #4965, .F. ) ;
#15398 = CARTESIAN_POINT ( 'NONE',  ( -5.842945980534647532, 1.369128644668957451, 17.12621569129737154 ) ) ;
#15399 = FACE_BOUND ( 'NONE', #4649, .T. ) ;
#15400 = DIRECTION ( 'NONE',  ( 0.000000000000000000, 0.000000000000000000, -1.000000000000000000 ) ) ;
#15401 = CARTESIAN_POINT ( 'NONE',  ( 2.500000000000000000, 3.061616997868383141E-16, -0.2999999999999999334 ) ) ;
#15402 = LINE ( 'NONE', #4741, #13268 ) ;
#15403 = CARTESIAN_POINT ( 'NONE',  ( 2.500000000000000000, 3.061616997868383141E-16, 1.400000002184949910 ) ) ;
#15404 = CARTESIAN_POINT ( 'NONE',  ( 1.035533905932738419, 185.3499999978151038, 9.500000000000003553 ) ) ;
#15405 = CARTESIAN_POINT ( 'NONE',  ( -1.454385272030960907, 228.7057613863525489, 8.277669994545302501 ) ) ;
#15406 = DIRECTION ( 'NONE',  ( 0.000000000000000000, 1.000000000000000000, 0.000000000000000000 ) ) ;
#15407 = CARTESIAN_POINT ( 'NONE',  ( 0.7995524673976757146, 6.199337389817257460, 25.11453679452471732 ) ) ;
#15408 = CARTESIAN_POINT ( 'NONE',  ( -1.461580736456472351, -1.461580736456473018, -0.2499999989075251672 ) ) ;
#15409 = CARTESIAN_POINT ( 'NONE',  ( -1.035533905932739751, 186.9499999999999886, 9.500000000000003553 ) ) ;
#15410 = CARTESIAN_POINT ( 'NONE',  ( 4.416397290909830353, -4.422724436066506115, 24.76379616840805653 ) ) ;
#15411 = CIRCLE ( 'NONE', #4231, 1.499999999999999556 ) ;
#15413 = ORIENTED_EDGE ( 'NONE', *, *, #8942, .F. ) ;
#15412 = CARTESIAN_POINT ( 'NONE',  ( 1.500000000000000000, 1.836970198721029934E-16, 2.500000000000000000 ) ) ;
#15414 = CARTESIAN_POINT ( 'NONE',  ( -4.435347140101074004, 4.403429997944469321, 5.000000000000004441 ) ) ;
#15415 = CARTESIAN_POINT ( 'NONE',  ( 0.000000000000000000, 0.000000000000000000, 52.97056274847714263 ) ) ;
#15416 = CARTESIAN_POINT ( 'NONE',  ( -2.753814924773092976, 227.6725260165826796, 8.454791258317579050 ) ) ;
#15417 =( LENGTH_UNIT ( ) NAMED_UNIT ( * ) SI_UNIT ( .MILLI., .METRE. ) );
#15418 = CARTESIAN_POINT ( 'NONE',  ( -1.767766952966368432, -1.767766952966369320, -0.4999999978150501123 ) ) ;
#15419 = DIRECTION ( 'NONE',  ( -0.9510565162951545304, 0.3090169943749447867, 0.000000000000000000 ) ) ;
#15420 = CARTESIAN_POINT ( 'NONE',  ( -0.7993282387950892964, 5.947240459526512701, 31.61484358216958057 ) ) ;
#15421 = APPLICATION_CONTEXT ( 'automotive_design' ) ;
#15422 = AXIS2_PLACEMENT_3D ( 'NONE', #3697, #1306, #4985 ) ;
#15423 = CARTESIAN_POINT ( 'NONE',  ( 0.6402346998162695701, 228.8776282932165600, 8.774031424212344277 ) ) ;
#15424 = CARTESIAN_POINT ( 'NONE',  ( 5.558508435838221295, 2.857531096718871844, 11.36762589283694247 ) ) ;
#15425 = CARTESIAN_POINT ( 'NONE',  ( -1.500000000000000000, -9.750000000000003553, 2.000000000000001776 ) ) ;
#15426 = VERTEX_POINT ( 'NONE', #1608 ) ;
#15427 = CARTESIAN_POINT ( 'NONE',  ( -1.461580736456473018, 185.3499999989074922, 5.538419263543526760 ) ) ;
#15428 = PRODUCT_DEFINITION_SHAPE ( 'NONE', 'NONE',  #15738 ) ;
#15429 = CARTESIAN_POINT ( 'NONE',  ( -2.500000000000000444, 184.4499999999999886, 8.035533905932737753 ) ) ;
#15430 = ADVANCED_FACE ( 'NONE', ( #7663 ), #499, .T. ) ;
#15431 = EDGE_CURVE ( 'NONE', #12139, #10038, #3085, .T. ) ;
#15432 = ORIENTED_EDGE ( 'NONE', *, *, #11511, .T. ) ;
#15433 = EDGE_CURVE ( 'NONE', #3038, #2035, #15234, .T. ) ;
#15434 = CARTESIAN_POINT ( 'NONE',  ( -2.668367453516630849, -5.373994336898132218, 5.000000000000004441 ) ) ;
#15435 = CARTESIAN_POINT ( 'NONE',  ( 2.500000000000000000, 3.061616997868383141E-16, -0.1999999978150501789 ) ) ;
#15436 = EDGE_CURVE ( 'NONE', #4624, #6402, #8017, .T. ) ;
#15437 = CARTESIAN_POINT ( 'NONE',  ( 4.416397290909816142, 4.422724436066522102, 17.73620383159193281 ) ) ;
#15438 = CARTESIAN_POINT ( 'NONE',  ( -1.461580736456473684, 185.5499999989075093, 8.461580736456474128 ) ) ;
#15439 = CARTESIAN_POINT ( 'NONE',  ( -4.344762547369660943, -4.493114738039267309, 5.503086438660448110 ) ) ;
#15440 = CARTESIAN_POINT ( 'NONE',  ( 2.500000000000000444, 1.035533905932737975, -0.9499999978150502900 ) ) ;
#15441 = FACE_OUTER_BOUND ( 'NONE', #7714, .T. ) ;
#15442 = CARTESIAN_POINT ( 'NONE',  ( -2.500000000000000000, 0.000000000000000000, 2.500000000000000000 ) ) ;
#15443 = CARTESIAN_POINT ( 'NONE',  ( 5.859155363331435495, -2.178872204144838509, 17.02599901976669017 ) ) ;
#15444 = CARTESIAN_POINT ( 'NONE',  ( 0.8002720181891173068, -6.199262377003402769, 30.38606262465556895 ) ) ;
#15445 = CARTESIAN_POINT ( 'NONE',  ( 3.796994071234844259E-16, -2.066987299999999639, -2.349999998907525089 ) ) ;
#15446 = CARTESIAN_POINT ( 'NONE',  ( -3.061616997868383141E-16, 189.0000000000000000, 7.000000000000000000 ) ) ;
#15447 =( REPRESENTATION_RELATIONSHIP ('NONE','NONE', #11191, #5305 ) REPRESENTATION_RELATIONSHIP_WITH_TRANSFORMATION ( #14818 )SHAPE_REPRESENTATION_RELATIONSHIP( ) );
#15448 = AXIS2_PLACEMENT_3D ( 'NONE', #14947, #7702, #9940 ) ;
#15449 = VERTEX_POINT ( 'NONE', #12433 ) ;
#15450 = ORIENTED_EDGE ( 'NONE', *, *, #13085, .T. ) ;
#15451 = ORIENTED_EDGE ( 'NONE', *, *, #5331, .T. ) ;
#15452 = CARTESIAN_POINT ( 'NONE',  ( 0.8561741729129461742, 185.0999999989075206, 9.066987299999999195 ) ) ;
#15453 = CARTESIAN_POINT ( 'NONE',  ( 0.5183317123408758276, 227.6299956641393294, 5.170797231135993322 ) ) ;
#15454 = VERTEX_POINT ( 'NONE', #5204 ) ;
#15455 = CARTESIAN_POINT ( 'NONE',  ( -1.035533905932737753, 2.500000000000000444, 1.650000002184949910 ) ) ;
#15456 = AXIS2_PLACEMENT_3D ( 'NONE', #3236, #11748, #11817 ) ;
#15457 = CARTESIAN_POINT ( 'NONE',  ( 0.9740807849836119470, -5.920620690450689949, 4.738501197006694809 ) ) ;
#15458 = CARTESIAN_POINT ( 'NONE',  ( 3.459597053047676507, 5.206576120509858185, 25.47408542334170889 ) ) ;
#15459 = CARTESIAN_POINT ( 'NONE',  ( 2.500000000000000000, 189.4999999978150527, 7.000000000000000000 ) ) ;
#15460 = CARTESIAN_POINT ( 'NONE',  ( -2.500000000000000444, 1.035533905932737753, -0.7430000000218497380 ) ) ;
#15461 = CYLINDRICAL_SURFACE ( 'NONE', #9741, 0.9999999999999998890 ) ;
#15462 = CARTESIAN_POINT ( 'NONE',  ( 2.066987299999999639, 0.8561741729129456191, 0.9000000010924746885 ) ) ;
#15463 = CARTESIAN_POINT ( 'NONE',  ( -2.500000000000000888, 189.2199999975965738, 8.035533905932737753 ) ) ;
#15464 = CARTESIAN_POINT ( 'NONE',  ( -0.1984404311693547251, 226.3267777912124075, 4.491376718485652120 ) ) ;
#15465 = DIRECTION ( 'NONE',  ( -0.000000000000000000, 1.000000000000000000, -0.000000000000000000 ) ) ;
#15466 = CIRCLE ( 'NONE', #8354, 1.499999999999999556 ) ;
#15467 = ADVANCED_FACE ( 'NONE', ( #2814 ), #13782, .F. ) ;
#15468 = AXIS2_PLACEMENT_3D ( 'NONE', #11375, #14886, #7955 ) ;
#15469 = ORIENTED_EDGE ( 'NONE', *, *, #5331, .F. ) ;
#15470 = CARTESIAN_POINT ( 'NONE',  ( -1.035533905932739751, 188.4499999978150697, 9.500000000000000000 ) ) ;
#15471 =( BOUNDED_SURFACE ( )  B_SPLINE_SURFACE ( 3, 2, ( 
 ( #998, #8498, #14271 ),
 ( #2183, #915, #6022 ),
 ( #13249, #5941, #9519 ),
 ( #11972, #7217, #3462 ),
 ( #10866, #9441, #14608 ),
 ( #13166, #10708, #15493 ),
 ( #4827, #12134, #11889 ),
 ( #6982, #11811, #2265 ),
 ( #1235, #10944, #15645 ),
 ( #7137, #43, #4589 ),
 ( #1078, #4908, #13326 ),
 ( #2428, #14843, #13720 ),
 ( #277, #5140, #7598 ),
 ( #14767, #356, #14686 ),
 ( #6340, #13558, #13406 ),
 ( #7520, #5304, #12287 ),
 ( #121, #11176, #1308 ),
 ( #12365, #9993, #12211 ),
 ( #12446, #3928, #1464 ),
 ( #7369, #5061, #11334 ),
 ( #13633, #6499, #4011 ),
 ( #2668, #1623, #431 ),
 ( #8576, #8804, #6421 ),
 ( #6183, #12524, #11022 ),
 ( #2748, #14919, #1546 ),
 ( #4986, #3775, #11255 ),
 ( #8888, #9836, #5222 ),
 ( #10070, #2828, #7676 ),
 ( #10150, #15004, #2515 ),
 ( #8652, #13483, #2587 ),
 ( #7442, #200, #1386 ),
 ( #6261, #11099, #9914 ) ),
 .UNSPECIFIED., .F., .F., .F. ) 
 B_SPLINE_SURFACE_WITH_KNOTS ( ( 4, 2, 2, 2, 2, 2, 2, 2, 2, 2, 2, 2, 2, 2, 2, 4 ),
 ( 3, 3 ),
 ( 0.006495126007820955193, 0.006901071383536445600, 0.007307016759251935140, 0.007712962134967425547, 0.008118907510682915954, 0.008524852886398405494, 0.008930798262113896768, 0.009742689013544875848, 0.01014863438926036539, 0.01055457976497585493, 0.01096052514069134620, 0.01136647051640683574, 0.01177241589212232528, 0.01217836126783781656, 0.01258430664355330610, 0.01299025201926879564 ),
 ( 0.000000000000000000, 1.000000000000000000 ),
 .UNSPECIFIED. ) 
 GEOMETRIC_REPRESENTATION_ITEM ( )  RATIONAL_B_SPLINE_SURFACE ( (
 ( 1.000000000000000000, 0.8259116554769078133, 1.000000000000000000),
 ( 1.000000000000000000, 0.8257451403044092642, 1.000000000000000000),
 ( 1.000000000000000000, 0.8262262825652272324, 1.000000000000000000),
 ( 1.000000000000000000, 0.8282882085239741121, 1.000000000000000000),
 ( 1.000000000000000000, 0.8298670479083970486, 1.000000000000000000),
 ( 1.000000000000000000, 0.8338618467773711851, 1.000000000000000000),
 ( 1.000000000000000000, 0.8362196290431722634, 1.000000000000000000),
 ( 1.000000000000000000, 0.8411780429153195016, 1.000000000000000000),
 ( 1.000000000000000000, 0.8438131714200759470, 1.000000000000000000),
 ( 1.000000000000000000, 0.8487328695746524376, 1.000000000000000000),
 ( 1.000000000000000000, 0.8510248968242735135, 1.000000000000000000),
 ( 1.000000000000000000, 0.8549300986948997760, 1.000000000000000000),
 ( 1.000000000000000000, 0.8565209868850615083, 1.000000000000000000),
 ( 1.000000000000000000, 0.8598120940792107758, 1.000000000000000000),
 ( 1.000000000000000000, 0.8600061557766143228, 1.000000000000000000),
 ( 1.000000000000000000, 0.8577564625823946853, 1.000000000000000000),
 ( 1.000000000000000000, 0.8565991989799338624, 1.000000000000000000),
 ( 1.000000000000000000, 0.8537317661690416726, 1.000000000000000000),
 ( 1.000000000000000000, 0.8520458150393346308, 1.000000000000000000),
 ( 1.000000000000000000, 0.8483981972192249366, 1.000000000000000000),
 ( 1.000000000000000000, 0.8464144394435542118, 1.000000000000000000),
 ( 1.000000000000000000, 0.8424405162120318646, 1.000000000000000000),
 ( 1.000000000000000000, 0.8404672314583410131, 1.000000000000000000),
 ( 1.000000000000000000, 0.8366782202000002666, 1.000000000000000000),
 ( 1.000000000000000000, 0.8348411284253109965, 1.000000000000000000),
 ( 1.000000000000000000, 0.8315664188806370927, 1.000000000000000000),
 ( 1.000000000000000000, 0.8301207044443068561, 1.000000000000000000),
 ( 1.000000000000000000, 0.8276856662744687121, 1.000000000000000000),
 ( 1.000000000000000000, 0.8267013226302402096, 1.000000000000000000),
 ( 1.000000000000000000, 0.8253456704432764468, 1.000000000000000000),
 ( 1.000000000000000000, 0.8249566822916403197, 1.000000000000000000),
 ( 1.000000000000000000, 0.8248771365966394153, 1.000000000000000000) ) ) 
 REPRESENTATION_ITEM ( '' )  SURFACE ( )  );
#15472 = ORIENTED_EDGE ( 'NONE', *, *, #12905, .T. ) ;
#15473 = CARTESIAN_POINT ( 'NONE',  ( 1.000082492230738085, 6.169467968613703057, 31.13152538105391898 ) ) ;
#15474 = SURFACE_SIDE_STYLE ('',( #7564 ) ) ;
#15475 = CARTESIAN_POINT ( 'NONE',  ( 7.347881242120658060E-16, 6.000000000000000888, 4.000000000000004441 ) ) ;
#15476 = EDGE_CURVE ( 'NONE', #14884, #15154, #14470, .T. ) ;
#15477 = EDGE_LOOP ( 'NONE', ( #8771, #2450, #3969, #1646 ) ) ;
#15478 = CARTESIAN_POINT ( 'NONE',  ( -5.621278735166202800, 2.101423246382537968, 17.02591947216897950 ) ) ;
#15479 = CARTESIAN_POINT ( 'NONE',  ( 7.347880431581855163E-16, -6.250000000000000888, 4.000000000000004441 ) ) ;
#15480 = EDGE_CURVE ( 'NONE', #3549, #3604, #5322, .T. ) ;
#15481 = CIRCLE ( 'NONE', #5825, 5.000000000000000000 ) ;
#15482 = FACE_BOUND ( 'NONE', #12158, .T. ) ;
#15483 = DIRECTION ( 'NONE',  ( 0.000000000000000000, 0.000000000000000000, 1.000000000000000000 ) ) ;
#15484 = MANIFOLD_SOLID_BREP ( 'AdvancedHole2', #11562 ) ;
#15485 = CARTESIAN_POINT ( 'NONE',  ( -1.035533905932737753, 2.500000000000000444, 0.7500000000000001110 ) ) ;
#15486 = CARTESIAN_POINT ( 'NONE',  ( -2.849573632035199644, -5.280958870664642646, 31.61561732698606875 ) ) ;
#15487 = SURFACE_SIDE_STYLE ('',( #13000 ) ) ;
#15488 = CARTESIAN_POINT ( 'NONE',  ( 0.000000000000000000, 0.4000000000000062395, -2.450963827680254337 ) ) ;
#15489 =( BOUNDED_CURVE ( )  B_SPLINE_CURVE ( 2, ( #14306, #3415, #11928, #8286, #13120, #5897, #10744, #15603, #12402 ),
 .UNSPECIFIED., .F., .F. ) 
 B_SPLINE_CURVE_WITH_KNOTS ( ( 3, 2, 2, 2, 3 ),
 ( 0.07142857142857141073, 0.08928571428571427382, 0.1071428571428571230, 0.1250000000000000000, 0.1428571428571428492 ),
 .UNSPECIFIED. ) 
 CURVE ( )  GEOMETRIC_REPRESENTATION_ITEM ( )  RATIONAL_B_SPLINE_CURVE ( ( 1.000000000000000000, 0.9238795325112866275, 1.000000000000000000, 0.9238795325112867385, 1.000000000000000000, 0.9238795325112867385, 1.000000000000000000, 0.9238795325112867385, 1.000000000000000000 ) ) 
 REPRESENTATION_ITEM ( '' )  );
#15490 = CARTESIAN_POINT ( 'NONE',  ( -2.500000000000000444, 185.8999999978150584, 7.000000000000000000 ) ) ;
#15491 = CARTESIAN_POINT ( 'NONE',  ( 0.7764192831524953098, 228.2223555856212442, 10.07190823357606213 ) ) ;
#15492 = CARTESIAN_POINT ( 'NONE',  ( 5.782895619916161856, 1.604017620858061655, 10.52591947216897594 ) ) ;
#15493 = CARTESIAN_POINT ( 'NONE',  ( -1.304415936767590489, 190.0585524576826799, 4.499160646538907571 ) ) ;
#15494 = CIRCLE ( 'NONE', #7817, 20.00000000000000000 ) ;
#15495 = CARTESIAN_POINT ( 'NONE',  ( 1.767766952966368432, 187.8999999999999773, 8.767766952966368876 ) ) ;
#15496 = CARTESIAN_POINT ( 'NONE',  ( -3.779082820360838646, 4.979770177899141004, 25.50004906876532473 ) ) ;
#15498 = ORIENTED_EDGE ( 'NONE', *, *, #5166, .F. ) ;
#15497 = CARTESIAN_POINT ( 'NONE',  ( 1.767766952966368654, 1.767766952966369098, -1.699999997815050179 ) ) ;
#15499 = CARTESIAN_POINT ( 'NONE',  ( -6.172552660730974416, 0.9821660343538980431, 18.26379616840806008 ) ) ;
#15500 = CARTESIAN_POINT ( 'NONE',  ( 1.035533905932737753, 186.5499999999999829, 4.500000000000001776 ) ) ;
#15501 = CARTESIAN_POINT ( 'NONE',  ( -2.361157410827141145, 226.6937665785872014, 5.572992748502056948 ) ) ;
#15502 = CARTESIAN_POINT ( 'NONE',  ( 5.726049995854515906, 2.506679546901768418, 25.29954462468842991 ) ) ;
#15503 = CARTESIAN_POINT ( 'NONE',  ( 1.767766952966369320, 184.8300000002185186, 5.232233047033630235 ) ) ;
#15504 = LINE ( 'NONE', #4683, #14922 ) ;
#15505 = CARTESIAN_POINT ( 'NONE',  ( 0.8799020092372641377, 228.8451675208714562, 8.680282862240067843 ) ) ;
#15506 = FACE_BOUND ( 'NONE', #9100, .T. ) ;
#15507 = CARTESIAN_POINT ( 'NONE',  ( -2.066987299999999639, 0.8561741729129455081, 0.6000000010924748661 ) ) ;
#15508 = PLANE ( 'NONE',  #11772 ) ;
#15509 = VERTEX_POINT ( 'NONE', #15064 ) ;
#15510 = CARTESIAN_POINT ( 'NONE',  ( -5.558508435838095174, -2.857531096719115649, 24.49999999999999289 ) ) ;
#15511 = DIRECTION ( 'NONE',  ( -0.000000000000000000, 1.000000000000000000, -0.000000000000000000 ) ) ;
#15512 = ORIENTED_EDGE ( 'NONE', *, *, #6612, .F. ) ;
#15513 = CARTESIAN_POINT ( 'NONE',  ( 7.490007020835728113, -2.433650805992114918, 17.99999999999998934 ) ) ;
#15514 = ADVANCED_FACE ( 'NONE', ( #9177 ), #9029, .F. ) ;
#15515 = CARTESIAN_POINT ( 'NONE',  ( -2.692215568229824108, 5.362327947133604944, 31.26229037835932090 ) ) ;
#15516 = CARTESIAN_POINT ( 'NONE',  ( 5.329945432499631153, 2.755769831645132228, 17.73770962164070397 ) ) ;
#15517 = CARTESIAN_POINT ( 'NONE',  ( -2.066987300000000527, 185.3999999989075889, 6.143825827087054492 ) ) ;
#15518 = CARTESIAN_POINT ( 'NONE',  ( 3.735808404764950463, -4.696639218303163332, 18.97398020122238549 ) ) ;
#15519 = CARTESIAN_POINT ( 'NONE',  ( -1.035533905932737753, 2.500000000000000444, -0.7499999978150503344 ) ) ;
#15520 = CARTESIAN_POINT ( 'NONE',  ( -5.615811513735010863, -2.743665920700458116, 4.496913561339539456 ) ) ;
#15521 = CARTESIAN_POINT ( 'NONE',  ( 0.000000000000000000, 222.7460571280668091, 12.08513476933103625 ) ) ;
#15522 = CARTESIAN_POINT ( 'NONE',  ( 4.435347140101073116, -4.403429997944470209, 5.000000000000004441 ) ) ;
#15523 = DIRECTION ( 'NONE',  ( 0.000000000000000000, 0.000000000000000000, -1.000000000000000000 ) ) ;
#15524 = CARTESIAN_POINT ( 'NONE',  ( 5.621197618055705725, 2.101623592078435188, 12.47398020122238016 ) ) ;
#15525 = EDGE_CURVE ( 'NONE', #320, #8616, #10680, .T. ) ;
#15526 = VERTEX_POINT ( 'NONE', #14911 ) ;
#15527 = VERTEX_POINT ( 'NONE', #8879 ) ;
#15528 = ORIENTED_EDGE ( 'NONE', *, *, #6785, .F. ) ;
#15529 = CARTESIAN_POINT ( 'NONE',  ( 4.290130679986543072, 4.545972905167758427, 30.38439807107077684 ) ) ;
#15530 = CARTESIAN_POINT ( 'NONE',  ( 1.500101834665445999, 227.8300896185262161, 5.748679984017036837 ) ) ;
#15531 = MANIFOLD_SOLID_BREP ( 'CirPattern1', #11307 ) ;
#15532 = EDGE_LOOP ( 'NONE', ( #14808, #6403, #4576, #723, #11371, #12256, #9397, #10710 ) ) ;
#15533 = VECTOR ( 'NONE', #9609, 1000.000000000000000 ) ;
#15534 = B_SPLINE_CURVE_WITH_KNOTS ( 'NONE', 3,
 ( #6795, #13707, #11324, #5520, #7821, #1612, #345, #6642, #12670, #10060, #12818, #14018, #5209, #3048, #13784, #11399, #8953, #5292 ),
 .UNSPECIFIED., .F., .F.,
 ( 4, 2, 2, 2, 2, 2, 2, 2, 4 ),
 ( 0.000000000000000000, 0.0003914357524127469435, 0.0007828715048254938870, 0.001174307257238240776, 0.001565743009650987774, 0.001957178762063734555, 0.002348614514476482420, 0.002740050266889230719, 0.003131486019301978150 ),
 .UNSPECIFIED. ) ;
#15535 = CARTESIAN_POINT ( 'NONE',  ( 0.8561741729129451750, 2.066987299999999639, 1.000000001092474555 ) ) ;
#15536 = CARTESIAN_POINT ( 'NONE',  ( 6.176542424588125968, 0.9554180641284963915, 17.99999999999998934 ) ) ;
#15537 = DIRECTION ( 'NONE',  ( 0.000000000000000000, 1.000000000000000000, 0.000000000000000000 ) ) ;
#15538 = CARTESIAN_POINT ( 'NONE',  ( 0.8561741729129460632, 186.6999999989075150, 9.066987299999999195 ) ) ;
#15539 = CARTESIAN_POINT ( 'NONE',  ( 1.767766952966369320, -1.767766952966368654, -1.193000000021849472 ) ) ;
#15540 = LINE ( 'NONE', #10602, #4393 ) ;
#15541 = EDGE_CURVE ( 'NONE', #1040, #6081, #5582, .T. ) ;
#15542 = ITEM_DEFINED_TRANSFORMATION ( 'NONE', 'NONE', #7380,  #14201 ) ;
#15543 = CARTESIAN_POINT ( 'NONE',  ( 0.8561741729129451750, 2.066987299999999639, -0.5999999989075250895 ) ) ;
#15544 = CARTESIAN_POINT ( 'NONE',  ( 3.254737477228069942, -5.337033878705166323, 4.126326713640079191 ) ) ;
#15545 = CARTESIAN_POINT ( 'NONE',  ( 1.751153496549405775, 226.5057898163625794, 5.019064844972819017 ) ) ;
#15546 = CARTESIAN_POINT ( 'NONE',  ( 3.779681992289694481, 4.979315417303977753, 18.99995078984292363 ) ) ;
#15547 = ORIENTED_EDGE ( 'NONE', *, *, #9136, .T. ) ;
#15548 = CARTESIAN_POINT ( 'NONE',  ( 0.000000000000000000, 184.0000000000000000, 7.000000000000000000 ) ) ;
#15549 = ORIENTED_EDGE ( 'NONE', *, *, #15588, .T. ) ;
#15550 = EDGE_LOOP ( 'NONE', ( #6404, #4451, #2250, #1277 ) ) ;
#15551 = CARTESIAN_POINT ( 'NONE',  ( -6.142844459177213778, 1.156093792145326260, 25.11560192892921606 ) ) ;
#15552 = CARTESIAN_POINT ( 'NONE',  ( 1.353717517954364224E-13, -6.250000000000000888, 17.99999999999998934 ) ) ;
#15553 = CARTESIAN_POINT ( 'NONE',  ( 2.094888798833199608E-14, -6.000000000000000888, 30.00000000000000000 ) ) ;
#15554 = ORIENTED_EDGE ( 'NONE', *, *, #10587, .T. ) ;
#15555 = EDGE_CURVE ( 'NONE', #9501, #302, #6414, .T. ) ;
#15556 = CARTESIAN_POINT ( 'NONE',  ( -5.858813228503671588, 2.179803269293220325, 31.97377282875268989 ) ) ;
#15557 = CARTESIAN_POINT ( 'NONE',  ( -0.2637975869347825020, -6.245592211692892803, 5.973328399491914631 ) ) ;
#15558 = FACE_BOUND ( 'NONE', #11621, .T. ) ;
#15559 = CARTESIAN_POINT ( 'NONE',  ( -1.767766952966369098, 1.767766952966369098, -2.399999999999999911 ) ) ;
#15560 = DIRECTION ( 'NONE',  ( 0.000000000000000000, 0.000000000000000000, -1.000000000000000000 ) ) ;
#15561 = CARTESIAN_POINT ( 'NONE',  ( 0.000000000000000000, 0.000000000000000000, 0.000000000000000000 ) ) ;
#15562 = CARTESIAN_POINT ( 'NONE',  ( 1.767766952966369098, 187.9999999978150527, 5.232233047033630235 ) ) ;
#15563 = CARTESIAN_POINT ( 'NONE',  ( 1.625192428541204714, 228.1012562471100011, 9.715842694323066908 ) ) ;
#15564 = CARTESIAN_POINT ( 'NONE',  ( 5.558508435838291462, -2.857531096718732400, 17.99999999999998934 ) ) ;
#15565 = ADVANCED_FACE ( 'NONE', ( #8797 ), #8040, .F. ) ;
#15566 =( BOUNDED_CURVE ( )  B_SPLINE_CURVE ( 2, ( #2765, #6277, #373, #13739, #4112, #12463, #3869, #6592, #1565, #7773, #15096, #10087, #6441, #1482, #14938 ),
 .UNSPECIFIED., .F., .F. ) 
 B_SPLINE_CURVE_WITH_KNOTS ( ( 3, 2, 2, 2, 2, 2, 2, 3 ),
 ( 0.7678571432794594198, 0.7857142857142856984, 0.8035714285714286031, 0.8214285714285713969, 0.8392857142857143016, 0.8571428571428570953, 0.8750000000000000000, 0.8928571428571429047 ),
 .UNSPECIFIED. ) 
 CURVE ( )  GEOMETRIC_REPRESENTATION_ITEM ( )  RATIONAL_B_SPLINE_CURVE ( ( 1.000000000000000000, 0.9238795325112867385, 1.000000000000000000, 0.9238795325112867385, 1.000000000000000000, 0.9238795325112867385, 1.000000000000000000, 0.9238795325112867385, 1.000000000000000000, 0.9238795325112867385, 1.000000000000000000, 0.9238795325112867385, 1.000000000000000000, 0.9238795325112867385, 1.000000000000000000 ) ) 
 REPRESENTATION_ITEM ( '' )  );
#15567 = CARTESIAN_POINT ( 'NONE',  ( 5.375913338529070273, 2.664979843780479030, 31.50428920362020335 ) ) ;
#15568 = VECTOR ( 'NONE', #7379, 1000.000000000000000 ) ;
#15569 = ORIENTED_EDGE ( 'NONE', *, *, #11916, .T. ) ;
#15570 = CARTESIAN_POINT ( 'NONE',  ( 7.799024015210693328, -1.482594289696895551, 24.49999999999999289 ) ) ;
#15571 = CARTESIAN_POINT ( 'NONE',  ( 0.1306497350717998329, -6.000000000000000888, 10.49999999999998224 ) ) ;
#15573 = VERTEX_POINT ( 'NONE', #7591 ) ;
#15572 = CARTESIAN_POINT ( 'NONE',  ( 1.767766952966368654, 1.767766952966369098, -1.000000000000000000 ) ) ;
#15574 = LINE ( 'NONE', #8582, #4296 ) ;
#15575 = CARTESIAN_POINT ( 'NONE',  ( 0.000000000000000000, 19.99999999999999645, 0.000000000000000000 ) ) ;
#15576 = CARTESIAN_POINT ( 'NONE',  ( -1.461580736456472351, -1.461580736456473018, -2.649999998907525356 ) ) ;
#15577 = CARTESIAN_POINT ( 'NONE',  ( -2.066987299999999639, 0.8561741729129452860, 0.6000000010924748661 ) ) ;
#15578 = CARTESIAN_POINT ( 'NONE',  ( -2.534040306409066190, 227.8072189287023832, 8.851078430691819321 ) ) ;
#15579 = CARTESIAN_POINT ( 'NONE',  ( 0.3078036515352236546, 189.4415565186901347, 3.987496826561411911 ) ) ;
#15580 = CARTESIAN_POINT ( 'NONE',  ( -2.500000000000000444, 185.8800000002185300, 5.964466094067261359 ) ) ;
#15581 = CARTESIAN_POINT ( 'NONE',  ( -2.931156713028464811, 5.520271803279225509, 5.504369696801525436 ) ) ;
#15582 = CARTESIAN_POINT ( 'NONE',  ( -0.8818726034074957365, 227.6760006002180319, 5.303662110480990677 ) ) ;
#15583 = DIRECTION ( 'NONE',  ( 0.000000000000000000, 0.000000000000000000, -1.000000000000000000 ) ) ;
#15584 = CARTESIAN_POINT ( 'NONE',  ( 2.066987300000000083, -0.8561741729129450640, 1.800000001092475044 ) ) ;
#15585 = CARTESIAN_POINT ( 'NONE',  ( 0.9737778612005694168, 5.920671847850513814, 30.73736375884650585 ) ) ;
#15586 = VERTEX_POINT ( 'NONE', #2819 ) ;
#15587 = CARTESIAN_POINT ( 'NONE',  ( 1.461580736456472573, 187.3499999989074922, 8.461580736456474128 ) ) ;
#15588 = EDGE_CURVE ( 'NONE', #3604, #3549, #8644, .T. ) ;
#15589 = CARTESIAN_POINT ( 'NONE',  ( 0.8561741729129457301, 185.9999999989074979, 4.933012699999999029 ) ) ;
#15590 = CARTESIAN_POINT ( 'NONE',  ( 5.782895619916200936, 1.604017620857918436, 23.52591947216898305 ) ) ;
#15591 = EDGE_LOOP ( 'NONE', ( #14825, #4249 ) ) ;
#15592 = VECTOR ( 'NONE', #14645, 1000.000000000000000 ) ;
#15593 = B_SPLINE_CURVE_WITH_KNOTS ( 'NONE', 3,
 ( #4373, #9231, #14546, #3567, #141, #4692, #1177, #7161, #9859, #8673, #11998, #12078, #6131, #5006, #15669, #3485, #9709, #3643 ),
 .UNSPECIFIED., .F., .F.,
 ( 4, 2, 2, 2, 2, 2, 2, 2, 4 ),
 ( 0.003131486019301968609, 0.003522824630466677917, 0.003914163241631387659, 0.004305501852796097401, 0.004696840463960805408, 0.005088179075125514282, 0.005479517686290222289, 0.005870856297454931164, 0.006262194908619639171 ),
 .UNSPECIFIED. ) ;
#15594 = CYLINDRICAL_SURFACE ( 'NONE', #3793, 1.499999999999999556 ) ;
#15595 = CARTESIAN_POINT ( 'NONE',  ( 5.317509234263971152, -2.779225709350972906, 5.132393880016354437 ) ) ;
#15596 = CARTESIAN_POINT ( 'NONE',  ( -4.143041610105363759, 4.340967609746979150, 31.61397738943081492 ) ) ;
#15597 = CARTESIAN_POINT ( 'NONE',  ( 6.780834061396424457E-14, 6.250000000000000888, 10.49999999999998224 ) ) ;
#15598 = CARTESIAN_POINT ( 'NONE',  ( -2.066987300000000527, 186.9999999989075263, 6.143825827087054492 ) ) ;
#15599 = CARTESIAN_POINT ( 'NONE',  ( 4.267936573529280686, -4.217499624512167422, 30.73770962164067200 ) ) ;
#15600 = CARTESIAN_POINT ( 'NONE',  ( 2.500000000000000000, 3.061616997868383141E-16, -1.799999997815050490 ) ) ;
#15601 = CARTESIAN_POINT ( 'NONE',  ( -6.250000000000000888, 0.000000000000000000, 36.00000000000000711 ) ) ;
#15602 = CARTESIAN_POINT ( 'NONE',  ( 1.767766952966369320, 184.0999999999999943, 5.232233047033630235 ) ) ;
#15603 = CARTESIAN_POINT ( 'NONE',  ( 2.500000000000000444, 185.4499999978150981, 8.035533905932739529 ) ) ;
#15604 = VECTOR ( 'NONE', #1658, 1000.000000000000000 ) ;
#15605 = CARTESIAN_POINT ( 'NONE',  ( -0.01285886373251123212, 189.6977690162252941, 10.38967773564543684 ) ) ;
#15606 = ADVANCED_FACE ( 'NONE', ( #11327 ), #11246, .F. ) ;
#15607 = ORIENTED_EDGE ( 'NONE', *, *, #4301, .T. ) ;
#15608 = ORIENTED_EDGE ( 'NONE', *, *, #7820, .T. ) ;
#15609 = ORIENTED_EDGE ( 'NONE', *, *, #68, .F. ) ;
#15610 = CARTESIAN_POINT ( 'NONE',  ( -0.0007128680628333008105, 227.6089742637946642, 5.110086227958842819 ) ) ;
#15611 = ORIENTED_EDGE ( 'NONE', *, *, #9262, .F. ) ;
#15612 = CARTESIAN_POINT ( 'NONE',  ( -1.767766952966368432, -1.767766952966369320, -2.099999997815050534 ) ) ;
#15613 = CARTESIAN_POINT ( 'NONE',  ( -0.5039079366030397855, 5.980031194523169447, 23.62637068109811977 ) ) ;
#15614 = CARTESIAN_POINT ( 'NONE',  ( 5.571002711501385818, 2.833546409886330775, 31.26379616840806719 ) ) ;
#15615 = CARTESIAN_POINT ( 'NONE',  ( 1.461580736456472351, 187.5499999989075093, 8.461580736456474128 ) ) ;
#15616 = CARTESIAN_POINT ( 'NONE',  ( 1.767766952966368654, 1.767766952966369098, 0.6069999999781504618 ) ) ;
#15617 = DIRECTION ( 'NONE',  ( 1.000000000000000000, 0.000000000000000000, 0.000000000000000000 ) ) ;
#15618 = CARTESIAN_POINT ( 'NONE',  ( -0.8561741729129458411, -2.066987299999999195, -2.599999998907525534 ) ) ;
#15619 = CARTESIAN_POINT ( 'NONE',  ( 4.322356511625540243, 7.650514973136639973, 17.99999999999998934 ) ) ;
#15620 = CARTESIAN_POINT ( 'NONE',  ( -0.1001789588503840533, 226.3251931448050698, 4.486704830075608719 ) ) ;
#15621 = LINE ( 'NONE', #7114, #7494 ) ;
#15622 = VERTEX_POINT ( 'NONE', #5212 ) ;
#15623 = ORIENTED_EDGE ( 'NONE', *, *, #11739, .T. ) ;
#15624 = LINE ( 'NONE', #1135, #9353 ) ;
#15625 = ORIENTED_EDGE ( 'NONE', *, *, #734, .T. ) ;
#15626 = EDGE_LOOP ( 'NONE', ( #4766, #12829, #12019, #10250 ) ) ;
#15627 = CARTESIAN_POINT ( 'NONE',  ( 0.2623718222035403280, 6.245654667075782207, 30.02627829713834728 ) ) ;
#15628 = VECTOR ( 'NONE', #2213, 1000.000000000000114 ) ;
#15629 = EDGE_CURVE ( 'NONE', #12014, #1272, #12299, .T. ) ;
#15630 = CARTESIAN_POINT ( 'NONE',  ( -3.882673863916357160, -4.899192824800883805, 23.52591457665828401 ) ) ;
#15631 = DIRECTION ( 'NONE',  ( -1.000000000000000000, 3.326610055774637112E-18, 1.062480551894331163E-17 ) ) ;
#15632 = EDGE_CURVE ( 'NONE', #7444, #25, #5181, .T. ) ;
#15633 = CARTESIAN_POINT ( 'NONE',  ( 3.106366801612014950, -5.134708448381275048, 12.37303779027049799 ) ) ;
#15634 = B_SPLINE_CURVE_WITH_KNOTS ( 'NONE', 3,
 ( #10751, #2073, #13294, #6947, #9647, #7099, #14488, #14400, #14165, #5749, #9402, #3507, #3586, #6068, #4629, #8459, #3346, #7180 ),
 .UNSPECIFIED., .F., .F.,
 ( 4, 2, 2, 2, 2, 2, 2, 2, 4 ),
 ( 0.000000000000000000, 0.0003914898357794970073, 0.0007829796715589940146, 0.001174469507338490913, 0.001565959343117988029, 0.001957449178897484928, 0.002348939014676983128, 0.002740428850456480894, 0.003131918686235978661 ),
 .UNSPECIFIED. ) ;
#15635 = CARTESIAN_POINT ( 'NONE',  ( -0.6156133477426863898, -6.220296490279942248, 5.798723873455115196 ) ) ;
#15636 = CARTESIAN_POINT ( 'NONE',  ( -0.6156133477424821088, -6.220296490279960011, 25.29872387345510987 ) ) ;
#15637 = DIRECTION ( 'NONE',  ( 0.000000000000000000, 0.000000000000000000, -1.000000000000000000 ) ) ;
#15638 = CARTESIAN_POINT ( 'NONE',  ( 5.782895619916152086, 1.604017620858103177, 30.02591947216899371 ) ) ;
#15639 = CARTESIAN_POINT ( 'NONE',  ( -3.459447313391949663, -5.206669755180918457, 25.47400098023329562 ) ) ;
#15640 = DIRECTION ( 'NONE',  ( 0.000000000000000000, -1.000000000000000000, 0.000000000000000000 ) ) ;
#15641 = CARTESIAN_POINT ( 'NONE',  ( -1.767766952966369765, 187.5999999978150754, 8.767766952966368876 ) ) ;
#15642 = AXIS2_PLACEMENT_3D ( 'NONE', #14985, #4076, #8947 ) ;
#15643 = CARTESIAN_POINT ( 'NONE',  ( 2.993808330938719564, 227.3535049858431591, 7.515946948957763496 ) ) ;
#15644 = CARTESIAN_POINT ( 'NONE',  ( 4.142173849413740783, 4.341773579105408842, 31.61519382448851090 ) ) ;
#15645 = CARTESIAN_POINT ( 'NONE',  ( -1.972033150788811806, 190.0185192967513501, 4.950362254874026036 ) ) ;
#15646 = ORIENTED_EDGE ( 'NONE', *, *, #12732, .T. ) ;
#15647 = CARTESIAN_POINT ( 'NONE',  ( -3.923477796648561888, 4.541042560386441274, 4.126962209729494901 ) ) ;
#15648 = CARTESIAN_POINT ( 'NONE',  ( 0.8736516769107610658, -5.936271176698223684, 10.99606771578675612 ) ) ;
#15650 = ORIENTED_EDGE ( 'NONE', *, *, #5238, .F. ) ;
#15649 = CARTESIAN_POINT ( 'NONE',  ( 5.747343991580224021, 1.727858744772142741, 25.49992002356261622 ) ) ;
#15651 = CARTESIAN_POINT ( 'NONE',  ( 0.1306171417090646603, 5.999999999999993783, 23.49999999999999289 ) ) ;
#15652 = CARTESIAN_POINT ( 'NONE',  ( 1.734160753182337755, 226.5019027256826121, 5.007583146736123147 ) ) ;
#15653 = CARTESIAN_POINT ( 'NONE',  ( -4.416678568553646933, -4.422441866694312829, 31.26236973443874945 ) ) ;
#15654 = CARTESIAN_POINT ( 'NONE',  ( 2.066987299999999639, 0.8561741729129456191, 0.3000000010924747662 ) ) ;
#15655 = CARTESIAN_POINT ( 'NONE',  ( -2.766897257556299117, 227.6625976227142019, 8.425578970441488735 ) ) ;
#15656 = FILL_AREA_STYLE ('',( #14132 ) ) ;
#15657 = CARTESIAN_POINT ( 'NONE',  ( -6.172552660730985963, 0.9821660343538300975, 11.76379616840804943 ) ) ;
#15658 = CARTESIAN_POINT ( 'NONE',  ( -1.035533905932739751, 186.8800000002184731, 9.500000000000003553 ) ) ;
#15659 = CARTESIAN_POINT ( 'NONE',  ( -3.567624405365297680, 5.133384272590741482, 5.999950789842938725 ) ) ;
#15660 = CARTESIAN_POINT ( 'NONE',  ( 1.052850409966403333, 227.7074407335792614, 5.394463008855642450 ) ) ;
#15661 = EDGE_CURVE ( 'NONE', #4525, #15318, #14095, .T. ) ;
#15662 = CARTESIAN_POINT ( 'NONE',  ( -2.692693252389608993, 5.362085866495096553, 30.73617396794405821 ) ) ;
#15663 = CARTESIAN_POINT ( 'NONE',  ( -1.461580736456472351, -1.461580736456473018, -0.04999999890752505893 ) ) ;
#15664 = CARTESIAN_POINT ( 'NONE',  ( 5.770331821586426102, 2.404225004693546275, 17.12619944752603729 ) ) ;
#15665 = ORIENTED_EDGE ( 'NONE', *, *, #7781, .F. ) ;
#15666 = CARTESIAN_POINT ( 'NONE',  ( 2.066987300000000083, 188.2499999989075263, 7.000000000000000000 ) ) ;
#15667 = ADVANCED_FACE ( 'NONE', ( #307 ), #14869, .F. ) ;
#15668 = CARTESIAN_POINT ( 'NONE',  ( 2.066987300000000971, 187.4999999989075548, 6.143825827087054492 ) ) ;
#15669 = CARTESIAN_POINT ( 'NONE',  ( -2.931212650151639565, -5.520239928492829407, 12.00425949503009093 ) ) ;
#15670 = ORIENTED_EDGE ( 'NONE', *, *, #14464, .T. ) ;
#15671 = CARTESIAN_POINT ( 'NONE',  ( -3.632151824461158363, -4.777505256984540871, 23.49995067926686687 ) ) ;
#15672 = B_SPLINE_CURVE_WITH_KNOTS ( 'NONE', 3,
 ( #10851, #9672, #10695, #15715, #13390, #14593, #4815, #15556, #13473, #11876, #4655, #9508, #1296, #14342, #3608, #8316, #32, #419 ),
 .UNSPECIFIED., .F., .F.,
 ( 4, 2, 2, 2, 2, 2, 2, 2, 4 ),
 ( 0.003131486019301988125, 0.003522824630466695264, 0.003914163241631402404, 0.004305501852796108676, 0.004696840463960815816, 0.005088179075125522956, 0.005479517686290229228, 0.005870856297454936368, 0.006262194908619643507 ),
 .UNSPECIFIED. ) ;
#15673 = DIRECTION ( 'NONE',  ( 0.000000000000000000, 0.000000000000000000, -1.000000000000000000 ) ) ;
#15674 = EDGE_CURVE ( 'NONE', #10771, #5182, #15494, .T. ) ;
#15675 = CYLINDRICAL_SURFACE ( 'NONE', #5688, 5.000000000000000000 ) ;
#15676 = CARTESIAN_POINT ( 'NONE',  ( 5.999999999999999112, 189.3270225533669020, 3.938484906660877805 ) ) ;
#15677 = CARTESIAN_POINT ( 'NONE',  ( -2.066987300000000971, 187.0999999989075206, 7.856174172912944620 ) ) ;
#15678 = CARTESIAN_POINT ( 'NONE',  ( 2.782468714962443190, -5.316055268221400176, 30.49610204984016448 ) ) ;
#15679 = CARTESIAN_POINT ( 'NONE',  ( 0.8615349496598407875, 189.0583051017248977, 10.06290867563976654 ) ) ;
#15680 = LINE ( 'NONE', #4942, #4787 ) ;
#15681 = CARTESIAN_POINT ( 'NONE',  ( -6.000000000000000888, 0.000000000000000000, 0.000000000000000000 ) ) ;
#15682 = CARTESIAN_POINT ( 'NONE',  ( -1.767766952966369320, 188.9999999978150527, 5.232233047033630235 ) ) ;
#15683 = CARTESIAN_POINT ( 'NONE',  ( 5.317509234263932960, 2.779225709351047069, 4.867606119983654445 ) ) ;
#15684 = ORIENTED_EDGE ( 'NONE', *, *, #11062, .F. ) ;
#15685 = EDGE_LOOP ( 'NONE', ( #6262, #2727, #685, #8654 ) ) ;
#15686 = AXIS2_PLACEMENT_3D ( 'NONE', #7309, #1248, #6123 ) ;
#15687 = ORIENTED_EDGE ( 'NONE', *, *, #14615, .F. ) ;
#15688 = B_SPLINE_CURVE_WITH_KNOTS ( 'NONE', 3,
 ( #2675, #5949, #15653, #284, #5466, #1706, #10158, #12373, #12610, #5231, #15086, #1554, #13802, #13731, #2837, #15012, #6352, #12455 ),
 .UNSPECIFIED., .F., .F.,
 ( 4, 2, 2, 2, 2, 2, 2, 2, 4 ),
 ( 0.003131486019301990293, 0.003522824630466696565, 0.003914163241631402404, 0.004305501852796108676, 0.004696840463960814949, 0.005088179075125520354, 0.005479517686290227493, 0.005870856297454932898, 0.006262194908619639171 ),
 .UNSPECIFIED. ) ;
#15689 = CARTESIAN_POINT ( 'NONE',  ( 1.727282114035952443, 228.5870706176066278, 7.934884284728715542 ) ) ;
#15690 = VERTEX_POINT ( 'NONE', #5563 ) ;
#15691 = CARTESIAN_POINT ( 'NONE',  ( 1.767766952966368654, 1.767766952966369098, -1.699999997815050401 ) ) ;
#15692 = CARTESIAN_POINT ( 'NONE',  ( 5.859155363331417732, 2.178872204144886471, 18.97400098023329562 ) ) ;
#15693 = AXIS2_PLACEMENT_3D ( 'NONE', #1693, #10144, #12361 ) ;
#15694 = CARTESIAN_POINT ( 'NONE',  ( 6.081836621194427472, 1.445163676684881882, 31.87305891554300530 ) ) ;
#15695 = CARTESIAN_POINT ( 'NONE',  ( 0.8561741729129452860, 188.5999999989074922, 4.933012699999999029 ) ) ;
#15696 = CARTESIAN_POINT ( 'NONE',  ( -2.500000000000000000, -1.035533905932739307, 0.1569999999781505062 ) ) ;
#15697 = AXIS2_PLACEMENT_3D ( 'NONE', #11204, #12392, #2854 ) ;
#15698 = CARTESIAN_POINT ( 'NONE',  ( -8.185202263645752375E-31, 182.0000000000000000, -9.500000000000000000 ) ) ;
#15699 = ITEM_DEFINED_TRANSFORMATION ( 'NONE', 'NONE', #15005,  #14201 ) ;
#15700 = CARTESIAN_POINT ( 'NONE',  ( -1.265664690411614835E-16, 2.066987299999999639, -1.349999998907525534 ) ) ;
#15701 = CARTESIAN_POINT ( 'NONE',  ( 3.568242062701590722, -5.132954954975464723, 29.99995093123466816 ) ) ;
#15702 = CARTESIAN_POINT ( 'NONE',  ( -1.240485740468941556, 226.4108687305035232, 4.739277288743133809 ) ) ;
#15703 = DIRECTION ( 'NONE',  ( -0.000000000000000000, -1.000000000000000000, -0.000000000000000000 ) ) ;
#15704 = VERTEX_POINT ( 'NONE', #7783 ) ;
#15705 = VERTEX_POINT ( 'NONE', #10409 ) ;
#15706 = CARTESIAN_POINT ( 'NONE',  ( -7.352245982167326943E-16, 188.4999999978150527, 9.500000000000001776 ) ) ;
#15707 = AXIS2_PLACEMENT_3D ( 'NONE', #15548, #2247, #14332 ) ;
#15708 = ORIENTED_EDGE ( 'NONE', *, *, #2897, .F. ) ;
#15709 = VERTEX_POINT ( 'NONE', #10254 ) ;
#15710 = CARTESIAN_POINT ( 'NONE',  ( -6.172552660730978857, -0.9821660343538717308, 30.73620383159192571 ) ) ;
#15711 = CIRCLE ( 'NONE', #10123, 2.500000000000000000 ) ;
#15712 = CARTESIAN_POINT ( 'NONE',  ( 3.421280866381102292, -4.930711975950938353, 16.99995067926686687 ) ) ;
#15713 = B_SPLINE_CURVE_WITH_KNOTS ( 'NONE', 3,
 ( #8180, #13096, #4281, #14053, #3318, #5561, #15182, #3161, #2039, #8018, #2193, #12856, #613, #924, #1961, #689, #10329, #7937 ),
 .UNSPECIFIED., .F., .F.,
 ( 4, 2, 2, 2, 2, 2, 2, 2, 4 ),
 ( 0.000000000000000000, 0.0003914898357794970615, 0.0007829796715589941230, 0.001174469507338491130, 0.001565959343117988246, 0.001957449178897485362, 0.002348939014676982261, 0.002740428850456479593, 0.003131918686235976492 ),
 .UNSPECIFIED. ) ;
#15714 = CARTESIAN_POINT ( 'NONE',  ( -3.736532060718080306, -4.696070028785897854, 25.47377823943292796 ) ) ;
#15715 = CARTESIAN_POINT ( 'NONE',  ( -5.615811513735035732, 2.743665920700399496, 31.50308643866046054 ) ) ;
#15716 = B_SPLINE_CURVE_WITH_KNOTS ( 'NONE', 3,
 ( #7298, #3626, #14526, #12291, #3548, #2353, #6265, #11027, #15649, #12215, #8332, #13411, #12138, #2519, #14612, #1239, #13331, #6111 ),
 .UNSPECIFIED., .F., .F.,
 ( 4, 2, 2, 2, 2, 2, 2, 2, 4 ),
 ( 0.003131918686235976058, 0.003523310662250265460, 0.003914702638264554863, 0.004306094614278844698, 0.004697486590293134534, 0.005088878566307424370, 0.005480270542321714206, 0.005871662518336003174, 0.006263054494350293010 ),
 .UNSPECIFIED. ) ;
#15717 = UNCERTAINTY_MEASURE_WITH_UNIT (LENGTH_MEASURE( 1.000000000000000082E-05 ), #11873, 'distance_accuracy_value', 'NONE');
#15718 = CARTESIAN_POINT ( 'NONE',  ( -0.8730628416137191650, -6.188929913094963986, 4.495049298931171222 ) ) ;
#15719 = CARTESIAN_POINT ( 'NONE',  ( -3.634089073485423427, -4.776071126502695385, 12.49992002356259313 ) ) ;
#15720 = CARTESIAN_POINT ( 'NONE',  ( -4.000000000000001776, 184.0000000000000000, 7.000000000000000888 ) ) ;
#15721 = MANIFOLD_SOLID_BREP ( 'Slot', #7508 ) ;
#15722 = CARTESIAN_POINT ( 'NONE',  ( 5.866817325727495813, 1.260653813892030017, 30.19977782616120621 ) ) ;
#15723 = FACE_OUTER_BOUND ( 'NONE', #14341, .T. ) ;
#15724 = CARTESIAN_POINT ( 'NONE',  ( 0.000000000000000000, 64.00000000000000000, 0.000000000000000000 ) ) ;
#15725 = VECTOR ( 'NONE', #4155, 1000.000000000000000 ) ;
#15726 = CARTESIAN_POINT ( 'NONE',  ( -7.352245982167326943E-16, 188.4999999978150527, 9.500000000000001776 ) ) ;
#15727 = AXIS2_PLACEMENT_3D ( 'NONE', #12188, #2319, #7192 ) ;
#15728 = CARTESIAN_POINT ( 'NONE',  ( 2.691218579993890803, 227.7172414894967858, 8.586351398698511161 ) ) ;
#15729 = CARTESIAN_POINT ( 'NONE',  ( -2.940898392866930777E-15, 228.9118723800512498, 8.872930300147352511 ) ) ;
#15730 = NEXT_ASSEMBLY_USAGE_OCCURRENCE ( 'NAUO1', ' ', ' ', #15082, #15315, $ ) ;
#15731 = NEXT_ASSEMBLY_USAGE_OCCURRENCE ( 'NAUO2', ' ', ' ', #15082, #10321, $ ) ;
#15732 = NEXT_ASSEMBLY_USAGE_OCCURRENCE ( 'NAUO3', ' ', ' ', #15082, #3028, $ ) ;
#15733 = NEXT_ASSEMBLY_USAGE_OCCURRENCE ( 'NAUO4', ' ', ' ', #15082, #10321, $ ) ;
#15734 = NEXT_ASSEMBLY_USAGE_OCCURRENCE ( 'NAUO5', ' ', ' ', #15082, #13615, $ ) ;
#15735 = NEXT_ASSEMBLY_USAGE_OCCURRENCE ( 'NAUO6', ' ', ' ', #15082, #13615, $ ) ;
#15736 = NEXT_ASSEMBLY_USAGE_OCCURRENCE ( 'NAUO7', ' ', ' ', #15082, #14597, $ ) ;
#15737 = NEXT_ASSEMBLY_USAGE_OCCURRENCE ( 'NAUO8', ' ', ' ', #15082, #6346, $ ) ;
#15738 = NEXT_ASSEMBLY_USAGE_OCCURRENCE ( 'NAUO9', ' ', ' ', #15082, #6346, $ ) ;
#15739 = NEXT_ASSEMBLY_USAGE_OCCURRENCE ( 'NAUO10', ' ', ' ', #15082, #6346, $ ) ;
#15740 = NEXT_ASSEMBLY_USAGE_OCCURRENCE ( 'NAUO11', ' ', ' ', #15082, #6346, $ ) ;
#15741 = NEXT_ASSEMBLY_USAGE_OCCURRENCE ( 'NAUO12', ' ', ' ', #15082, #13615, $ ) ;
#15742 = NEXT_ASSEMBLY_USAGE_OCCURRENCE ( 'NAUO13', ' ', ' ', #15082, #13615, $ ) ;
#15743 = NEXT_ASSEMBLY_USAGE_OCCURRENCE ( 'NAUO14', ' ', ' ', #15082, #13615, $ ) ;
#15744 = NEXT_ASSEMBLY_USAGE_OCCURRENCE ( 'NAUO15', ' ', ' ', #15082, #14597, $ ) ;
#15745 = NEXT_ASSEMBLY_USAGE_OCCURRENCE ( 'NAUO16', ' ', ' ', #15082, #14597, $ ) ;
#15746 = NEXT_ASSEMBLY_USAGE_OCCURRENCE ( 'NAUO17', ' ', ' ', #15082, #14597, $ ) ;
#15747 = NEXT_ASSEMBLY_USAGE_OCCURRENCE ( 'NAUO18', ' ', ' ', #15082, #6346, $ ) ;
#15748 = NEXT_ASSEMBLY_USAGE_OCCURRENCE ( 'NAUO19', ' ', ' ', #15082, #6346, $ ) ;
#15749 = NEXT_ASSEMBLY_USAGE_OCCURRENCE ( 'NAUO20', ' ', ' ', #15082, #6346, $ ) ;
#15750 = NEXT_ASSEMBLY_USAGE_OCCURRENCE ( 'NAUO21', ' ', ' ', #15082, #13615, $ ) ;
#15751 = NEXT_ASSEMBLY_USAGE_OCCURRENCE ( 'NAUO22', ' ', ' ', #15082, #13615, $ ) ;
#15752 = NEXT_ASSEMBLY_USAGE_OCCURRENCE ( 'NAUO23', ' ', ' ', #15082, #13615, $ ) ;
#15753 = NEXT_ASSEMBLY_USAGE_OCCURRENCE ( 'NAUO24', ' ', ' ', #15082, #6346, $ ) ;
#15754 = NEXT_ASSEMBLY_USAGE_OCCURRENCE ( 'NAUO25', ' ', ' ', #15082, #6346, $ ) ;
#15755 = NEXT_ASSEMBLY_USAGE_OCCURRENCE ( 'NAUO26', ' ', ' ', #15082, #6346, $ ) ;
#15756 = NEXT_ASSEMBLY_USAGE_OCCURRENCE ( 'NAUO27', ' ', ' ', #15082, #6346, $ ) ;
#15757 = NEXT_ASSEMBLY_USAGE_OCCURRENCE ( 'NAUO28', ' ', ' ', #15082, #6346, $ ) ;
#15758 = NEXT_ASSEMBLY_USAGE_OCCURRENCE ( 'NAUO29', ' ', ' ', #15082, #6346, $ ) ;
#15759 = NEXT_ASSEMBLY_USAGE_OCCURRENCE ( 'NAUO30', ' ', ' ', #15082, #6346, $ ) ;
#15760 = NEXT_ASSEMBLY_USAGE_OCCURRENCE ( 'NAUO31', ' ', ' ', #15082, #6346, $ ) ;
#15761 = NEXT_ASSEMBLY_USAGE_OCCURRENCE ( 'NAUO32', ' ', ' ', #15082, #6346, $ ) ;
#15762 = NEXT_ASSEMBLY_USAGE_OCCURRENCE ( 'NAUO33', ' ', ' ', #15082, #3310, $ ) ;
#15763 = NEXT_ASSEMBLY_USAGE_OCCURRENCE ( 'NAUO34', ' ', ' ', #15082, #6346, $ ) ;
#15764 = NEXT_ASSEMBLY_USAGE_OCCURRENCE ( 'NAUO35', ' ', ' ', #15082, #6346, $ ) ;
#15765 = NEXT_ASSEMBLY_USAGE_OCCURRENCE ( 'NAUO36', ' ', ' ', #15082, #2335, $ ) ;
#15766 = NEXT_ASSEMBLY_USAGE_OCCURRENCE ( 'NAUO37', ' ', ' ', #15082, #2335, $ ) ;
#15767 = NEXT_ASSEMBLY_USAGE_OCCURRENCE ( 'NAUO38', ' ', ' ', #15082, #2335, $ ) ;
#15768 = NEXT_ASSEMBLY_USAGE_OCCURRENCE ( 'NAUO39', ' ', ' ', #15082, #2335, $ ) ;
ENDSEC;
END-ISO-10303-21;
